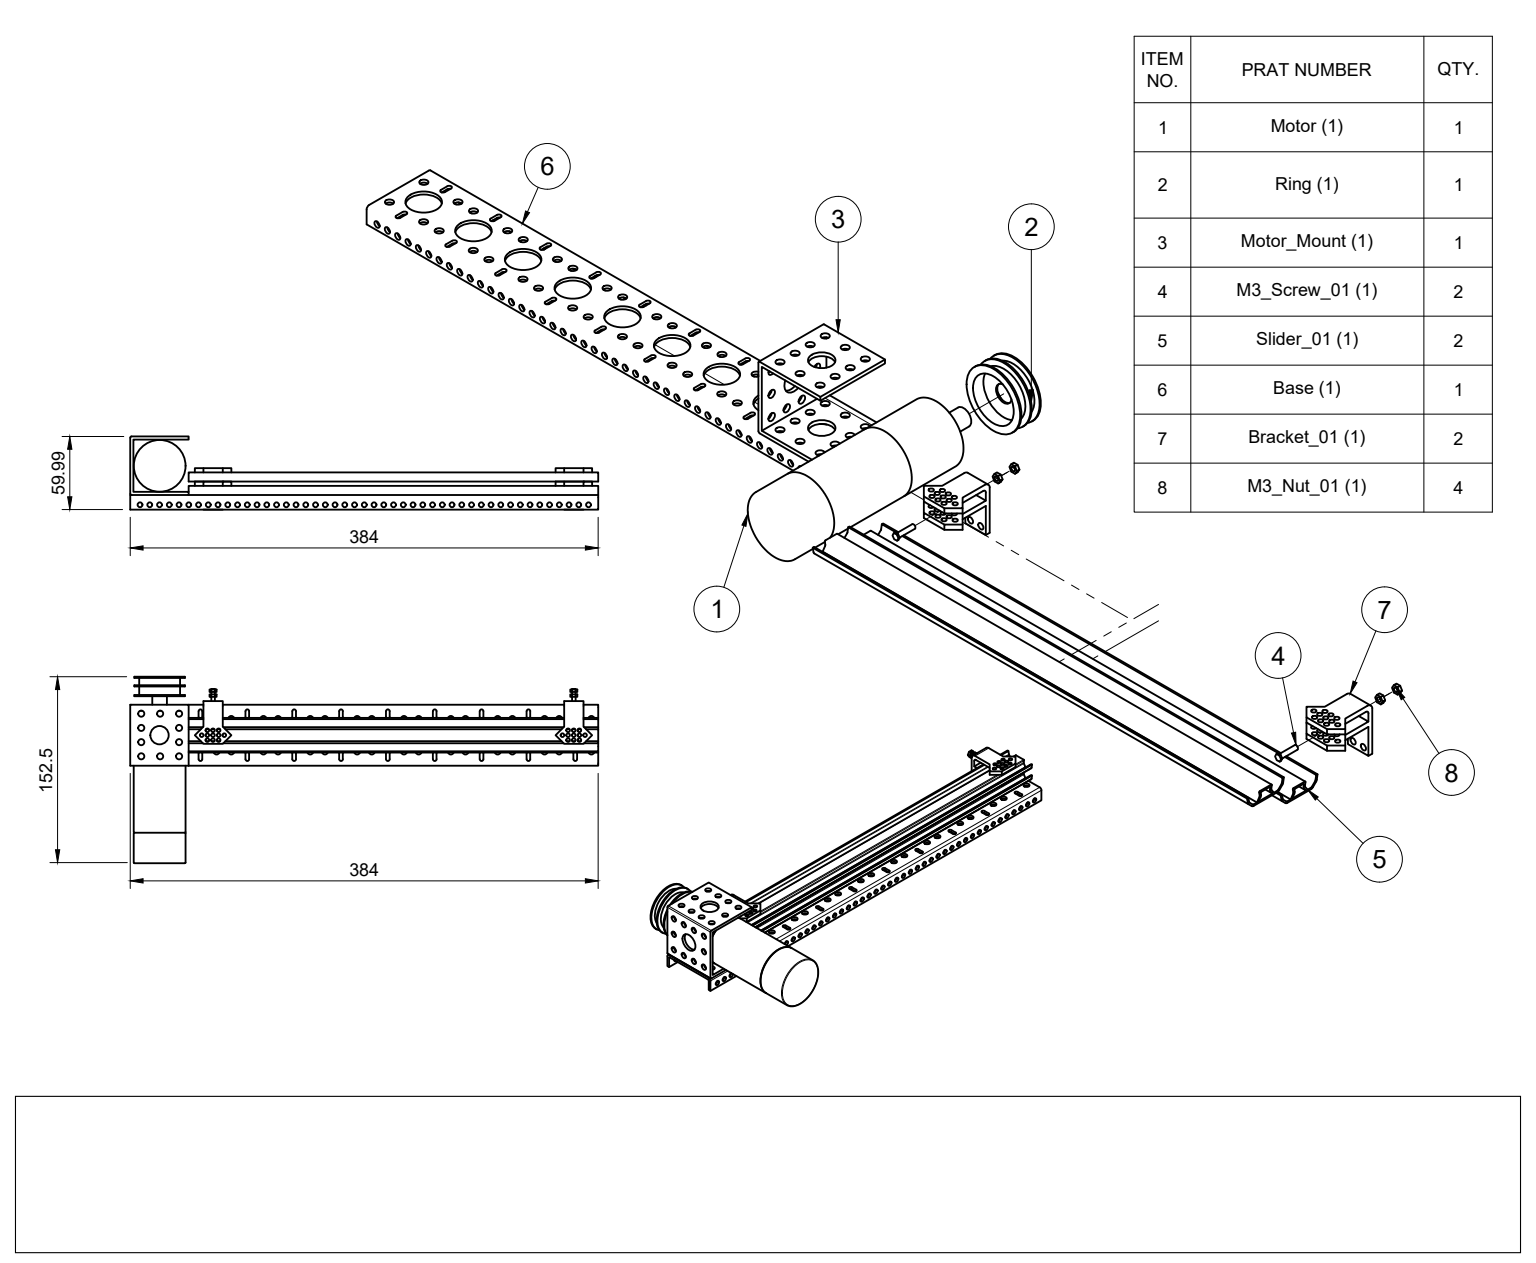
ISO-10303-21;
HEADER;
/* Generated by software containing ST-Developer
 * from STEP Tools, Inc. (www.steptools.com) 
 */

FILE_DESCRIPTION(
/* description */ (''),
/* implementation_level */ '2;1');

FILE_NAME(
/* name */ 'MAS-275',
/* time_stamp */ '2026-10-22T15:07:41+06:00',
/* author */ (''),
/* organization */ (''),
/* preprocessor_version */ 'ST-DEVELOPER v20.2',
/* originating_system */ 'Autodesk Translation Framework v15.15.0.0',
/* authorisation */ '');

FILE_SCHEMA (('AUTOMOTIVE_DESIGN { 1 0 10303 214 3 1 1 }'));
ENDSEC;

DATA;
#10=MECHANICAL_DESIGN_GEOMETRIC_PRESENTATION_REPRESENTATION('',(#2876,#2877,
#2878,#2879,#2880,#2881,#2882,#2883,#2884,#2885,#2886,#2887,#2888,#2889,
#2890,#2891),#19220);
#11=ITEM_DEFINED_TRANSFORMATION($,$,#11484,#12714);
#12=ITEM_DEFINED_TRANSFORMATION($,$,#11522,#12715);
#13=ITEM_DEFINED_TRANSFORMATION($,$,#11555,#12716);
#14=ITEM_DEFINED_TRANSFORMATION($,$,#11671,#12717);
#15=ITEM_DEFINED_TRANSFORMATION($,$,#11684,#12718);
#16=ITEM_DEFINED_TRANSFORMATION($,$,#11759,#12719);
#17=ITEM_DEFINED_TRANSFORMATION($,$,#12374,#12720);
#18=ITEM_DEFINED_TRANSFORMATION($,$,#12476,#12721);
#19=ITEM_DEFINED_TRANSFORMATION($,$,#12488,#12722);
#20=ITEM_DEFINED_TRANSFORMATION($,$,#12590,#12723);
#21=ITEM_DEFINED_TRANSFORMATION($,$,#12603,#12724);
#22=ITEM_DEFINED_TRANSFORMATION($,$,#12615,#12725);
#23=ITEM_DEFINED_TRANSFORMATION($,$,#12627,#12726);
#24=ITEM_DEFINED_TRANSFORMATION($,$,#12702,#12727);
#25=(
REPRESENTATION_RELATIONSHIP($,$,#19270,#19269)
REPRESENTATION_RELATIONSHIP_WITH_TRANSFORMATION(#11)
SHAPE_REPRESENTATION_RELATIONSHIP()
);
#26=(
REPRESENTATION_RELATIONSHIP($,$,#19271,#19269)
REPRESENTATION_RELATIONSHIP_WITH_TRANSFORMATION(#12)
SHAPE_REPRESENTATION_RELATIONSHIP()
);
#27=(
REPRESENTATION_RELATIONSHIP($,$,#19272,#19269)
REPRESENTATION_RELATIONSHIP_WITH_TRANSFORMATION(#13)
SHAPE_REPRESENTATION_RELATIONSHIP()
);
#28=(
REPRESENTATION_RELATIONSHIP($,$,#19273,#19269)
REPRESENTATION_RELATIONSHIP_WITH_TRANSFORMATION(#14)
SHAPE_REPRESENTATION_RELATIONSHIP()
);
#29=(
REPRESENTATION_RELATIONSHIP($,$,#19274,#19269)
REPRESENTATION_RELATIONSHIP_WITH_TRANSFORMATION(#15)
SHAPE_REPRESENTATION_RELATIONSHIP()
);
#30=(
REPRESENTATION_RELATIONSHIP($,$,#19275,#19269)
REPRESENTATION_RELATIONSHIP_WITH_TRANSFORMATION(#16)
SHAPE_REPRESENTATION_RELATIONSHIP()
);
#31=(
REPRESENTATION_RELATIONSHIP($,$,#19276,#19269)
REPRESENTATION_RELATIONSHIP_WITH_TRANSFORMATION(#17)
SHAPE_REPRESENTATION_RELATIONSHIP()
);
#32=(
REPRESENTATION_RELATIONSHIP($,$,#19277,#19269)
REPRESENTATION_RELATIONSHIP_WITH_TRANSFORMATION(#18)
SHAPE_REPRESENTATION_RELATIONSHIP()
);
#33=(
REPRESENTATION_RELATIONSHIP($,$,#19278,#19269)
REPRESENTATION_RELATIONSHIP_WITH_TRANSFORMATION(#19)
SHAPE_REPRESENTATION_RELATIONSHIP()
);
#34=(
REPRESENTATION_RELATIONSHIP($,$,#19279,#19269)
REPRESENTATION_RELATIONSHIP_WITH_TRANSFORMATION(#20)
SHAPE_REPRESENTATION_RELATIONSHIP()
);
#35=(
REPRESENTATION_RELATIONSHIP($,$,#19280,#19269)
REPRESENTATION_RELATIONSHIP_WITH_TRANSFORMATION(#21)
SHAPE_REPRESENTATION_RELATIONSHIP()
);
#36=(
REPRESENTATION_RELATIONSHIP($,$,#19281,#19269)
REPRESENTATION_RELATIONSHIP_WITH_TRANSFORMATION(#22)
SHAPE_REPRESENTATION_RELATIONSHIP()
);
#37=(
REPRESENTATION_RELATIONSHIP($,$,#19282,#19269)
REPRESENTATION_RELATIONSHIP_WITH_TRANSFORMATION(#23)
SHAPE_REPRESENTATION_RELATIONSHIP()
);
#38=(
REPRESENTATION_RELATIONSHIP($,$,#19283,#19269)
REPRESENTATION_RELATIONSHIP_WITH_TRANSFORMATION(#24)
SHAPE_REPRESENTATION_RELATIONSHIP()
);
#39=CONTEXT_DEPENDENT_SHAPE_REPRESENTATION(#25,#19255);
#40=CONTEXT_DEPENDENT_SHAPE_REPRESENTATION(#26,#19256);
#41=CONTEXT_DEPENDENT_SHAPE_REPRESENTATION(#27,#19257);
#42=CONTEXT_DEPENDENT_SHAPE_REPRESENTATION(#28,#19258);
#43=CONTEXT_DEPENDENT_SHAPE_REPRESENTATION(#29,#19259);
#44=CONTEXT_DEPENDENT_SHAPE_REPRESENTATION(#30,#19260);
#45=CONTEXT_DEPENDENT_SHAPE_REPRESENTATION(#31,#19261);
#46=CONTEXT_DEPENDENT_SHAPE_REPRESENTATION(#32,#19262);
#47=CONTEXT_DEPENDENT_SHAPE_REPRESENTATION(#33,#19263);
#48=CONTEXT_DEPENDENT_SHAPE_REPRESENTATION(#34,#19264);
#49=CONTEXT_DEPENDENT_SHAPE_REPRESENTATION(#35,#19265);
#50=CONTEXT_DEPENDENT_SHAPE_REPRESENTATION(#36,#19266);
#51=CONTEXT_DEPENDENT_SHAPE_REPRESENTATION(#37,#19267);
#52=CONTEXT_DEPENDENT_SHAPE_REPRESENTATION(#38,#19268);
#53=NEXT_ASSEMBLY_USAGE_OCCURRENCE('Motor (1):1','Motor (1):1',
'Motor (1):1',#19285,#19286,'Motor (1):1');
#54=NEXT_ASSEMBLY_USAGE_OCCURRENCE('Ring (1):1','Ring (1):1',
'Ring (1):1',#19285,#19287,'Ring (1):1');
#55=NEXT_ASSEMBLY_USAGE_OCCURRENCE('Motor_Mount (1):1',
'Motor_Mount (1):1','Motor_Mount (1):1',#19285,#19288,
'Motor_Mount (1):1');
#56=NEXT_ASSEMBLY_USAGE_OCCURRENCE('M3_Screw_01 (1):1',
'M3_Screw_01 (1):1','M3_Screw_01 (1):1',#19285,#19289,
'M3_Screw_01 (1):1');
#57=NEXT_ASSEMBLY_USAGE_OCCURRENCE('Slider_01 (1):1','Slider_01 (1):1',
'Slider_01 (1):1',#19285,#19290,'Slider_01 (1):1');
#58=NEXT_ASSEMBLY_USAGE_OCCURRENCE('Base (1):1','Base (1):1',
'Base (1):1',#19285,#19291,'Base (1):1');
#59=NEXT_ASSEMBLY_USAGE_OCCURRENCE('Bracket_01 (1):1',
'Bracket_01 (1):1','Bracket_01 (1):1',#19285,#19292,'Bracket_01 (1):1');
#60=NEXT_ASSEMBLY_USAGE_OCCURRENCE('M3_Nut_01 (1):1','M3_Nut_01 (1):1',
'M3_Nut_01 (1):1',#19285,#19293,'M3_Nut_01 (1):1');
#61=NEXT_ASSEMBLY_USAGE_OCCURRENCE('Bracket_02 (1):1',
'Bracket_02 (1):1','Bracket_02 (1):1',#19285,#19294,'Bracket_02 (1):1');
#62=NEXT_ASSEMBLY_USAGE_OCCURRENCE('M3_Screw_02 (1):1',
'M3_Screw_02 (1):1','M3_Screw_02 (1):1',#19285,#19295,
'M3_Screw_02 (1):1');
#63=NEXT_ASSEMBLY_USAGE_OCCURRENCE('M3_Nut_02 (1):1','M3_Nut_02 (1):1',
'M3_Nut_02 (1):1',#19285,#19296,'M3_Nut_02 (1):1');
#64=NEXT_ASSEMBLY_USAGE_OCCURRENCE('M3_Nut_03 (1):1','M3_Nut_03 (1):1',
'M3_Nut_03 (1):1',#19285,#19297,'M3_Nut_03 (1):1');
#65=NEXT_ASSEMBLY_USAGE_OCCURRENCE('Slider_02 (1):1','Slider_02 (1):1',
'Slider_02 (1):1',#19285,#19298,'Slider_02 (1):1');
#66=NEXT_ASSEMBLY_USAGE_OCCURRENCE('M3_Nut_04 (1):1','M3_Nut_04 (1):1',
'M3_Nut_04 (1):1',#19285,#19299,'M3_Nut_04 (1):1');
#67=SHAPE_REPRESENTATION_RELATIONSHIP('SRR','None',#19270,#81);
#68=SHAPE_REPRESENTATION_RELATIONSHIP('SRR','None',#19271,#82);
#69=SHAPE_REPRESENTATION_RELATIONSHIP('SRR','None',#19272,#83);
#70=SHAPE_REPRESENTATION_RELATIONSHIP('SRR','None',#19273,#84);
#71=SHAPE_REPRESENTATION_RELATIONSHIP('SRR','None',#19274,#85);
#72=SHAPE_REPRESENTATION_RELATIONSHIP('SRR','None',#19275,#86);
#73=SHAPE_REPRESENTATION_RELATIONSHIP('SRR','None',#19276,#87);
#74=SHAPE_REPRESENTATION_RELATIONSHIP('SRR','None',#19277,#88);
#75=SHAPE_REPRESENTATION_RELATIONSHIP('SRR','None',#19278,#89);
#76=SHAPE_REPRESENTATION_RELATIONSHIP('SRR','None',#19279,#90);
#77=SHAPE_REPRESENTATION_RELATIONSHIP('SRR','None',#19280,#91);
#78=SHAPE_REPRESENTATION_RELATIONSHIP('SRR','None',#19281,#92);
#79=SHAPE_REPRESENTATION_RELATIONSHIP('SRR','None',#19282,#93);
#80=SHAPE_REPRESENTATION_RELATIONSHIP('SRR','None',#19283,#94);
#81=ADVANCED_BREP_SHAPE_REPRESENTATION('',(#95),#19206);
#82=ADVANCED_BREP_SHAPE_REPRESENTATION('',(#96),#19207);
#83=ADVANCED_BREP_SHAPE_REPRESENTATION('',(#97),#19208);
#84=ADVANCED_BREP_SHAPE_REPRESENTATION('',(#98),#19209);
#85=ADVANCED_BREP_SHAPE_REPRESENTATION('',(#99),#19210);
#86=ADVANCED_BREP_SHAPE_REPRESENTATION('',(#100),#19211);
#87=ADVANCED_BREP_SHAPE_REPRESENTATION('',(#101),#19212);
#88=ADVANCED_BREP_SHAPE_REPRESENTATION('',(#102),#19213);
#89=ADVANCED_BREP_SHAPE_REPRESENTATION('',(#103),#19214);
#90=ADVANCED_BREP_SHAPE_REPRESENTATION('',(#104),#19215);
#91=ADVANCED_BREP_SHAPE_REPRESENTATION('',(#105),#19216);
#92=ADVANCED_BREP_SHAPE_REPRESENTATION('',(#106),#19217);
#93=ADVANCED_BREP_SHAPE_REPRESENTATION('',(#107),#19218);
#94=ADVANCED_BREP_SHAPE_REPRESENTATION('',(#108),#19219);
#95=MANIFOLD_SOLID_BREP('Motor',#11314);
#96=MANIFOLD_SOLID_BREP('Ring',#11315);
#97=MANIFOLD_SOLID_BREP('Motor_Mount',#11316);
#98=MANIFOLD_SOLID_BREP('M3_Screw_01',#11317);
#99=MANIFOLD_SOLID_BREP('Slider_01',#11318);
#100=MANIFOLD_SOLID_BREP('Base',#11319);
#101=MANIFOLD_SOLID_BREP('Bracket_01',#11320);
#102=MANIFOLD_SOLID_BREP('M3_Nut_01',#11321);
#103=MANIFOLD_SOLID_BREP('Bracket_02',#11322);
#104=MANIFOLD_SOLID_BREP('M3_Screw_02',#11323);
#105=MANIFOLD_SOLID_BREP('M3_Nut_02',#11324);
#106=MANIFOLD_SOLID_BREP('M3_Nut_03',#11325);
#107=MANIFOLD_SOLID_BREP('Slider_02',#11326);
#108=MANIFOLD_SOLID_BREP('M3_Nut_04',#11327);
#109=FACE_BOUND('',#3450,.T.);
#110=FACE_BOUND('',#3453,.T.);
#111=FACE_BOUND('',#3456,.T.);
#112=FACE_BOUND('',#3458,.T.);
#113=FACE_BOUND('',#3460,.T.);
#114=FACE_BOUND('',#3464,.T.);
#115=FACE_BOUND('',#3467,.T.);
#116=FACE_BOUND('',#3472,.T.);
#117=FACE_BOUND('',#3475,.T.);
#118=FACE_BOUND('',#3478,.T.);
#119=FACE_BOUND('',#3479,.T.);
#120=FACE_BOUND('',#3480,.T.);
#121=FACE_BOUND('',#3481,.T.);
#122=FACE_BOUND('',#3482,.T.);
#123=FACE_BOUND('',#3483,.T.);
#124=FACE_BOUND('',#3484,.T.);
#125=FACE_BOUND('',#3485,.T.);
#126=FACE_BOUND('',#3486,.T.);
#127=FACE_BOUND('',#3487,.T.);
#128=FACE_BOUND('',#3488,.T.);
#129=FACE_BOUND('',#3526,.T.);
#130=FACE_BOUND('',#3527,.T.);
#131=FACE_BOUND('',#3528,.T.);
#132=FACE_BOUND('',#3529,.T.);
#133=FACE_BOUND('',#3530,.T.);
#134=FACE_BOUND('',#3531,.T.);
#135=FACE_BOUND('',#3532,.T.);
#136=FACE_BOUND('',#3533,.T.);
#137=FACE_BOUND('',#3534,.T.);
#138=FACE_BOUND('',#3535,.T.);
#139=FACE_BOUND('',#3536,.T.);
#140=FACE_BOUND('',#3538,.T.);
#141=FACE_BOUND('',#3539,.T.);
#142=FACE_BOUND('',#3540,.T.);
#143=FACE_BOUND('',#3541,.T.);
#144=FACE_BOUND('',#3542,.T.);
#145=FACE_BOUND('',#3543,.T.);
#146=FACE_BOUND('',#3544,.T.);
#147=FACE_BOUND('',#3545,.T.);
#148=FACE_BOUND('',#3546,.T.);
#149=FACE_BOUND('',#3547,.T.);
#150=FACE_BOUND('',#3548,.T.);
#151=FACE_BOUND('',#3551,.T.);
#152=FACE_BOUND('',#3552,.T.);
#153=FACE_BOUND('',#3553,.T.);
#154=FACE_BOUND('',#3554,.T.);
#155=FACE_BOUND('',#3555,.T.);
#156=FACE_BOUND('',#3556,.T.);
#157=FACE_BOUND('',#3557,.T.);
#158=FACE_BOUND('',#3558,.T.);
#159=FACE_BOUND('',#3559,.T.);
#160=FACE_BOUND('',#3560,.T.);
#161=FACE_BOUND('',#3561,.T.);
#162=FACE_BOUND('',#3563,.T.);
#163=FACE_BOUND('',#3564,.T.);
#164=FACE_BOUND('',#3565,.T.);
#165=FACE_BOUND('',#3566,.T.);
#166=FACE_BOUND('',#3567,.T.);
#167=FACE_BOUND('',#3568,.T.);
#168=FACE_BOUND('',#3569,.T.);
#169=FACE_BOUND('',#3570,.T.);
#170=FACE_BOUND('',#3571,.T.);
#171=FACE_BOUND('',#3572,.T.);
#172=FACE_BOUND('',#3573,.T.);
#173=FACE_BOUND('',#3575,.T.);
#174=FACE_BOUND('',#3576,.T.);
#175=FACE_BOUND('',#3577,.T.);
#176=FACE_BOUND('',#3578,.T.);
#177=FACE_BOUND('',#3579,.T.);
#178=FACE_BOUND('',#3580,.T.);
#179=FACE_BOUND('',#3581,.T.);
#180=FACE_BOUND('',#3582,.T.);
#181=FACE_BOUND('',#3583,.T.);
#182=FACE_BOUND('',#3584,.T.);
#183=FACE_BOUND('',#3585,.T.);
#184=FACE_BOUND('',#3588,.T.);
#185=FACE_BOUND('',#3639,.T.);
#186=FACE_BOUND('',#3641,.T.);
#187=FACE_BOUND('',#3774,.T.);
#188=FACE_BOUND('',#3775,.T.);
#189=FACE_BOUND('',#3776,.T.);
#190=FACE_BOUND('',#3777,.T.);
#191=FACE_BOUND('',#3778,.T.);
#192=FACE_BOUND('',#3779,.T.);
#193=FACE_BOUND('',#3780,.T.);
#194=FACE_BOUND('',#3781,.T.);
#195=FACE_BOUND('',#3782,.T.);
#196=FACE_BOUND('',#3783,.T.);
#197=FACE_BOUND('',#3784,.T.);
#198=FACE_BOUND('',#3785,.T.);
#199=FACE_BOUND('',#3786,.T.);
#200=FACE_BOUND('',#3787,.T.);
#201=FACE_BOUND('',#3788,.T.);
#202=FACE_BOUND('',#3789,.T.);
#203=FACE_BOUND('',#3790,.T.);
#204=FACE_BOUND('',#3791,.T.);
#205=FACE_BOUND('',#3792,.T.);
#206=FACE_BOUND('',#3793,.T.);
#207=FACE_BOUND('',#3794,.T.);
#208=FACE_BOUND('',#3795,.T.);
#209=FACE_BOUND('',#3796,.T.);
#210=FACE_BOUND('',#3797,.T.);
#211=FACE_BOUND('',#3798,.T.);
#212=FACE_BOUND('',#3799,.T.);
#213=FACE_BOUND('',#3800,.T.);
#214=FACE_BOUND('',#3801,.T.);
#215=FACE_BOUND('',#3802,.T.);
#216=FACE_BOUND('',#3803,.T.);
#217=FACE_BOUND('',#3804,.T.);
#218=FACE_BOUND('',#3805,.T.);
#219=FACE_BOUND('',#3806,.T.);
#220=FACE_BOUND('',#3807,.T.);
#221=FACE_BOUND('',#3808,.T.);
#222=FACE_BOUND('',#3809,.T.);
#223=FACE_BOUND('',#3810,.T.);
#224=FACE_BOUND('',#3811,.T.);
#225=FACE_BOUND('',#3812,.T.);
#226=FACE_BOUND('',#3813,.T.);
#227=FACE_BOUND('',#3814,.T.);
#228=FACE_BOUND('',#3815,.T.);
#229=FACE_BOUND('',#3816,.T.);
#230=FACE_BOUND('',#3817,.T.);
#231=FACE_BOUND('',#3818,.T.);
#232=FACE_BOUND('',#3819,.T.);
#233=FACE_BOUND('',#3820,.T.);
#234=FACE_BOUND('',#3821,.T.);
#235=FACE_BOUND('',#3822,.T.);
#236=FACE_BOUND('',#3823,.T.);
#237=FACE_BOUND('',#3824,.T.);
#238=FACE_BOUND('',#3825,.T.);
#239=FACE_BOUND('',#3826,.T.);
#240=FACE_BOUND('',#3827,.T.);
#241=FACE_BOUND('',#3828,.T.);
#242=FACE_BOUND('',#3829,.T.);
#243=FACE_BOUND('',#3830,.T.);
#244=FACE_BOUND('',#3831,.T.);
#245=FACE_BOUND('',#3832,.T.);
#246=FACE_BOUND('',#3833,.T.);
#247=FACE_BOUND('',#3834,.T.);
#248=FACE_BOUND('',#3835,.T.);
#249=FACE_BOUND('',#3836,.T.);
#250=FACE_BOUND('',#3837,.T.);
#251=FACE_BOUND('',#3838,.T.);
#252=FACE_BOUND('',#3839,.T.);
#253=FACE_BOUND('',#3840,.T.);
#254=FACE_BOUND('',#3841,.T.);
#255=FACE_BOUND('',#3842,.T.);
#256=FACE_BOUND('',#3843,.T.);
#257=FACE_BOUND('',#3846,.T.);
#258=FACE_BOUND('',#3847,.T.);
#259=FACE_BOUND('',#3848,.T.);
#260=FACE_BOUND('',#3849,.T.);
#261=FACE_BOUND('',#3850,.T.);
#262=FACE_BOUND('',#3851,.T.);
#263=FACE_BOUND('',#3852,.T.);
#264=FACE_BOUND('',#3853,.T.);
#265=FACE_BOUND('',#3854,.T.);
#266=FACE_BOUND('',#3855,.T.);
#267=FACE_BOUND('',#3856,.T.);
#268=FACE_BOUND('',#3857,.T.);
#269=FACE_BOUND('',#3858,.T.);
#270=FACE_BOUND('',#3859,.T.);
#271=FACE_BOUND('',#3860,.T.);
#272=FACE_BOUND('',#3861,.T.);
#273=FACE_BOUND('',#3862,.T.);
#274=FACE_BOUND('',#3863,.T.);
#275=FACE_BOUND('',#3864,.T.);
#276=FACE_BOUND('',#3865,.T.);
#277=FACE_BOUND('',#3866,.T.);
#278=FACE_BOUND('',#3867,.T.);
#279=FACE_BOUND('',#3868,.T.);
#280=FACE_BOUND('',#3869,.T.);
#281=FACE_BOUND('',#3870,.T.);
#282=FACE_BOUND('',#3871,.T.);
#283=FACE_BOUND('',#3872,.T.);
#284=FACE_BOUND('',#3873,.T.);
#285=FACE_BOUND('',#3874,.T.);
#286=FACE_BOUND('',#3875,.T.);
#287=FACE_BOUND('',#3876,.T.);
#288=FACE_BOUND('',#3877,.T.);
#289=FACE_BOUND('',#3878,.T.);
#290=FACE_BOUND('',#3879,.T.);
#291=FACE_BOUND('',#3880,.T.);
#292=FACE_BOUND('',#3881,.T.);
#293=FACE_BOUND('',#3882,.T.);
#294=FACE_BOUND('',#3883,.T.);
#295=FACE_BOUND('',#3884,.T.);
#296=FACE_BOUND('',#3885,.T.);
#297=FACE_BOUND('',#3886,.T.);
#298=FACE_BOUND('',#3887,.T.);
#299=FACE_BOUND('',#3888,.T.);
#300=FACE_BOUND('',#3889,.T.);
#301=FACE_BOUND('',#3890,.T.);
#302=FACE_BOUND('',#3891,.T.);
#303=FACE_BOUND('',#3892,.T.);
#304=FACE_BOUND('',#3895,.T.);
#305=FACE_BOUND('',#3896,.T.);
#306=FACE_BOUND('',#3897,.T.);
#307=FACE_BOUND('',#3898,.T.);
#308=FACE_BOUND('',#3899,.T.);
#309=FACE_BOUND('',#3900,.T.);
#310=FACE_BOUND('',#3901,.T.);
#311=FACE_BOUND('',#3902,.T.);
#312=FACE_BOUND('',#3903,.T.);
#313=FACE_BOUND('',#3904,.T.);
#314=FACE_BOUND('',#3905,.T.);
#315=FACE_BOUND('',#3906,.T.);
#316=FACE_BOUND('',#3907,.T.);
#317=FACE_BOUND('',#3908,.T.);
#318=FACE_BOUND('',#3909,.T.);
#319=FACE_BOUND('',#3910,.T.);
#320=FACE_BOUND('',#3911,.T.);
#321=FACE_BOUND('',#3912,.T.);
#322=FACE_BOUND('',#3913,.T.);
#323=FACE_BOUND('',#3914,.T.);
#324=FACE_BOUND('',#3915,.T.);
#325=FACE_BOUND('',#3916,.T.);
#326=FACE_BOUND('',#3917,.T.);
#327=FACE_BOUND('',#3918,.T.);
#328=FACE_BOUND('',#3919,.T.);
#329=FACE_BOUND('',#3920,.T.);
#330=FACE_BOUND('',#3921,.T.);
#331=FACE_BOUND('',#3922,.T.);
#332=FACE_BOUND('',#3923,.T.);
#333=FACE_BOUND('',#3924,.T.);
#334=FACE_BOUND('',#3925,.T.);
#335=FACE_BOUND('',#3926,.T.);
#336=FACE_BOUND('',#3927,.T.);
#337=FACE_BOUND('',#3928,.T.);
#338=FACE_BOUND('',#3929,.T.);
#339=FACE_BOUND('',#3930,.T.);
#340=FACE_BOUND('',#3931,.T.);
#341=FACE_BOUND('',#3932,.T.);
#342=FACE_BOUND('',#3933,.T.);
#343=FACE_BOUND('',#3934,.T.);
#344=FACE_BOUND('',#3935,.T.);
#345=FACE_BOUND('',#3936,.T.);
#346=FACE_BOUND('',#3937,.T.);
#347=FACE_BOUND('',#3938,.T.);
#348=FACE_BOUND('',#3939,.T.);
#349=FACE_BOUND('',#3940,.T.);
#350=FACE_BOUND('',#3941,.T.);
#351=FACE_BOUND('',#3942,.T.);
#352=FACE_BOUND('',#3943,.T.);
#353=FACE_BOUND('',#3944,.T.);
#354=FACE_BOUND('',#3945,.T.);
#355=FACE_BOUND('',#3946,.T.);
#356=FACE_BOUND('',#3947,.T.);
#357=FACE_BOUND('',#3948,.T.);
#358=FACE_BOUND('',#3949,.T.);
#359=FACE_BOUND('',#3950,.T.);
#360=FACE_BOUND('',#3951,.T.);
#361=FACE_BOUND('',#3952,.T.);
#362=FACE_BOUND('',#3953,.T.);
#363=FACE_BOUND('',#3954,.T.);
#364=FACE_BOUND('',#3955,.T.);
#365=FACE_BOUND('',#3956,.T.);
#366=FACE_BOUND('',#3957,.T.);
#367=FACE_BOUND('',#3958,.T.);
#368=FACE_BOUND('',#3959,.T.);
#369=FACE_BOUND('',#3960,.T.);
#370=FACE_BOUND('',#3961,.T.);
#371=FACE_BOUND('',#3962,.T.);
#372=FACE_BOUND('',#3963,.T.);
#373=FACE_BOUND('',#3964,.T.);
#374=FACE_BOUND('',#4016,.T.);
#375=FACE_BOUND('',#4017,.T.);
#376=FACE_BOUND('',#4018,.T.);
#377=FACE_BOUND('',#4019,.T.);
#378=FACE_BOUND('',#4020,.T.);
#379=FACE_BOUND('',#4021,.T.);
#380=FACE_BOUND('',#4022,.T.);
#381=FACE_BOUND('',#4023,.T.);
#382=FACE_BOUND('',#4024,.T.);
#383=FACE_BOUND('',#4025,.T.);
#384=FACE_BOUND('',#4026,.T.);
#385=FACE_BOUND('',#4027,.T.);
#386=FACE_BOUND('',#4028,.T.);
#387=FACE_BOUND('',#4029,.T.);
#388=FACE_BOUND('',#4030,.T.);
#389=FACE_BOUND('',#4031,.T.);
#390=FACE_BOUND('',#4032,.T.);
#391=FACE_BOUND('',#4033,.T.);
#392=FACE_BOUND('',#4034,.T.);
#393=FACE_BOUND('',#4035,.T.);
#394=FACE_BOUND('',#4036,.T.);
#395=FACE_BOUND('',#4037,.T.);
#396=FACE_BOUND('',#4038,.T.);
#397=FACE_BOUND('',#4039,.T.);
#398=FACE_BOUND('',#4040,.T.);
#399=FACE_BOUND('',#4041,.T.);
#400=FACE_BOUND('',#4042,.T.);
#401=FACE_BOUND('',#4043,.T.);
#402=FACE_BOUND('',#4044,.T.);
#403=FACE_BOUND('',#4045,.T.);
#404=FACE_BOUND('',#4046,.T.);
#405=FACE_BOUND('',#4047,.T.);
#406=FACE_BOUND('',#4048,.T.);
#407=FACE_BOUND('',#4049,.T.);
#408=FACE_BOUND('',#4050,.T.);
#409=FACE_BOUND('',#4051,.T.);
#410=FACE_BOUND('',#4052,.T.);
#411=FACE_BOUND('',#4053,.T.);
#412=FACE_BOUND('',#4054,.T.);
#413=FACE_BOUND('',#4055,.T.);
#414=FACE_BOUND('',#4056,.T.);
#415=FACE_BOUND('',#4057,.T.);
#416=FACE_BOUND('',#4058,.T.);
#417=FACE_BOUND('',#4059,.T.);
#418=FACE_BOUND('',#4060,.T.);
#419=FACE_BOUND('',#4061,.T.);
#420=FACE_BOUND('',#4062,.T.);
#421=FACE_BOUND('',#4113,.T.);
#422=FACE_BOUND('',#4114,.T.);
#423=FACE_BOUND('',#4115,.T.);
#424=FACE_BOUND('',#4116,.T.);
#425=FACE_BOUND('',#4117,.T.);
#426=FACE_BOUND('',#4118,.T.);
#427=FACE_BOUND('',#4119,.T.);
#428=FACE_BOUND('',#4120,.T.);
#429=FACE_BOUND('',#4121,.T.);
#430=FACE_BOUND('',#4122,.T.);
#431=FACE_BOUND('',#4123,.T.);
#432=FACE_BOUND('',#4124,.T.);
#433=FACE_BOUND('',#4125,.T.);
#434=FACE_BOUND('',#4126,.T.);
#435=FACE_BOUND('',#4127,.T.);
#436=FACE_BOUND('',#4128,.T.);
#437=FACE_BOUND('',#4129,.T.);
#438=FACE_BOUND('',#4130,.T.);
#439=FACE_BOUND('',#4131,.T.);
#440=FACE_BOUND('',#4132,.T.);
#441=FACE_BOUND('',#4133,.T.);
#442=FACE_BOUND('',#4134,.T.);
#443=FACE_BOUND('',#4135,.T.);
#444=FACE_BOUND('',#4136,.T.);
#445=FACE_BOUND('',#4137,.T.);
#446=FACE_BOUND('',#4138,.T.);
#447=FACE_BOUND('',#4139,.T.);
#448=FACE_BOUND('',#4140,.T.);
#449=FACE_BOUND('',#4141,.T.);
#450=FACE_BOUND('',#4142,.T.);
#451=FACE_BOUND('',#4143,.T.);
#452=FACE_BOUND('',#4144,.T.);
#453=FACE_BOUND('',#4145,.T.);
#454=FACE_BOUND('',#4146,.T.);
#455=FACE_BOUND('',#4147,.T.);
#456=FACE_BOUND('',#4148,.T.);
#457=FACE_BOUND('',#4149,.T.);
#458=FACE_BOUND('',#4150,.T.);
#459=FACE_BOUND('',#4151,.T.);
#460=FACE_BOUND('',#4152,.T.);
#461=FACE_BOUND('',#4153,.T.);
#462=FACE_BOUND('',#4154,.T.);
#463=FACE_BOUND('',#4155,.T.);
#464=FACE_BOUND('',#4156,.T.);
#465=FACE_BOUND('',#4157,.T.);
#466=FACE_BOUND('',#4158,.T.);
#467=FACE_BOUND('',#4159,.T.);
#468=FACE_BOUND('',#4161,.T.);
#469=FACE_BOUND('',#4162,.T.);
#470=FACE_BOUND('',#4163,.T.);
#471=FACE_BOUND('',#4164,.T.);
#472=FACE_BOUND('',#4165,.T.);
#473=FACE_BOUND('',#4166,.T.);
#474=FACE_BOUND('',#4167,.T.);
#475=FACE_BOUND('',#4168,.T.);
#476=FACE_BOUND('',#4169,.T.);
#477=FACE_BOUND('',#4170,.T.);
#478=FACE_BOUND('',#4171,.T.);
#479=FACE_BOUND('',#4172,.T.);
#480=FACE_BOUND('',#4173,.T.);
#481=FACE_BOUND('',#4174,.T.);
#482=FACE_BOUND('',#4175,.T.);
#483=FACE_BOUND('',#4176,.T.);
#484=FACE_BOUND('',#4177,.T.);
#485=FACE_BOUND('',#4178,.T.);
#486=FACE_BOUND('',#4179,.T.);
#487=FACE_BOUND('',#4180,.T.);
#488=FACE_BOUND('',#4181,.T.);
#489=FACE_BOUND('',#4182,.T.);
#490=FACE_BOUND('',#4183,.T.);
#491=FACE_BOUND('',#4184,.T.);
#492=FACE_BOUND('',#4185,.T.);
#493=FACE_BOUND('',#4186,.T.);
#494=FACE_BOUND('',#4187,.T.);
#495=FACE_BOUND('',#4188,.T.);
#496=FACE_BOUND('',#4189,.T.);
#497=FACE_BOUND('',#4190,.T.);
#498=FACE_BOUND('',#4191,.T.);
#499=FACE_BOUND('',#4192,.T.);
#500=FACE_BOUND('',#4193,.T.);
#501=FACE_BOUND('',#4194,.T.);
#502=FACE_BOUND('',#4195,.T.);
#503=FACE_BOUND('',#4196,.T.);
#504=FACE_BOUND('',#4197,.T.);
#505=FACE_BOUND('',#4198,.T.);
#506=FACE_BOUND('',#4199,.T.);
#507=FACE_BOUND('',#4200,.T.);
#508=FACE_BOUND('',#4201,.T.);
#509=FACE_BOUND('',#4202,.T.);
#510=FACE_BOUND('',#4203,.T.);
#511=FACE_BOUND('',#4204,.T.);
#512=FACE_BOUND('',#4205,.T.);
#513=FACE_BOUND('',#4206,.T.);
#514=FACE_BOUND('',#4207,.T.);
#515=FACE_BOUND('',#4213,.T.);
#516=FACE_BOUND('',#4214,.T.);
#517=FACE_BOUND('',#4215,.T.);
#518=FACE_BOUND('',#4216,.T.);
#519=FACE_BOUND('',#4217,.T.);
#520=FACE_BOUND('',#4218,.T.);
#521=FACE_BOUND('',#4219,.T.);
#522=FACE_BOUND('',#4220,.T.);
#523=FACE_BOUND('',#4221,.T.);
#524=FACE_BOUND('',#4222,.T.);
#525=FACE_BOUND('',#4223,.T.);
#526=FACE_BOUND('',#4226,.T.);
#527=FACE_BOUND('',#4227,.T.);
#528=FACE_BOUND('',#4228,.T.);
#529=FACE_BOUND('',#4229,.T.);
#530=FACE_BOUND('',#4230,.T.);
#531=FACE_BOUND('',#4231,.T.);
#532=FACE_BOUND('',#4232,.T.);
#533=FACE_BOUND('',#4233,.T.);
#534=FACE_BOUND('',#4234,.T.);
#535=FACE_BOUND('',#4235,.T.);
#536=FACE_BOUND('',#4236,.T.);
#537=FACE_BOUND('',#4254,.T.);
#538=FACE_BOUND('',#4255,.T.);
#539=FACE_BOUND('',#4256,.T.);
#540=FACE_BOUND('',#4257,.T.);
#541=FACE_BOUND('',#4258,.T.);
#542=FACE_BOUND('',#4259,.T.);
#543=FACE_BOUND('',#4260,.T.);
#544=FACE_BOUND('',#4261,.T.);
#545=FACE_BOUND('',#4262,.T.);
#546=FACE_BOUND('',#4263,.T.);
#547=FACE_BOUND('',#4264,.T.);
#548=FACE_BOUND('',#4282,.T.);
#549=FACE_BOUND('',#4283,.T.);
#550=FACE_BOUND('',#4284,.T.);
#551=FACE_BOUND('',#4285,.T.);
#552=FACE_BOUND('',#4286,.T.);
#553=FACE_BOUND('',#4287,.T.);
#554=FACE_BOUND('',#4288,.T.);
#555=FACE_BOUND('',#4289,.T.);
#556=FACE_BOUND('',#4290,.T.);
#557=FACE_BOUND('',#4291,.T.);
#558=FACE_BOUND('',#4292,.T.);
#559=FACE_BOUND('',#4294,.T.);
#560=FACE_BOUND('',#4295,.T.);
#561=FACE_BOUND('',#4296,.T.);
#562=FACE_BOUND('',#4298,.T.);
#563=FACE_BOUND('',#4301,.T.);
#564=FACE_BOUND('',#4302,.T.);
#565=FACE_BOUND('',#4313,.T.);
#566=FACE_BOUND('',#4315,.T.);
#567=FACE_BOUND('',#4321,.T.);
#568=FACE_BOUND('',#4322,.T.);
#569=FACE_BOUND('',#4323,.T.);
#570=FACE_BOUND('',#4324,.T.);
#571=FACE_BOUND('',#4325,.T.);
#572=FACE_BOUND('',#4326,.T.);
#573=FACE_BOUND('',#4327,.T.);
#574=FACE_BOUND('',#4328,.T.);
#575=FACE_BOUND('',#4329,.T.);
#576=FACE_BOUND('',#4330,.T.);
#577=FACE_BOUND('',#4331,.T.);
#578=FACE_BOUND('',#4334,.T.);
#579=FACE_BOUND('',#4335,.T.);
#580=FACE_BOUND('',#4336,.T.);
#581=FACE_BOUND('',#4337,.T.);
#582=FACE_BOUND('',#4338,.T.);
#583=FACE_BOUND('',#4339,.T.);
#584=FACE_BOUND('',#4340,.T.);
#585=FACE_BOUND('',#4341,.T.);
#586=FACE_BOUND('',#4342,.T.);
#587=FACE_BOUND('',#4343,.T.);
#588=FACE_BOUND('',#4344,.T.);
#589=FACE_BOUND('',#4362,.T.);
#590=FACE_BOUND('',#4363,.T.);
#591=FACE_BOUND('',#4364,.T.);
#592=FACE_BOUND('',#4365,.T.);
#593=FACE_BOUND('',#4366,.T.);
#594=FACE_BOUND('',#4367,.T.);
#595=FACE_BOUND('',#4368,.T.);
#596=FACE_BOUND('',#4369,.T.);
#597=FACE_BOUND('',#4370,.T.);
#598=FACE_BOUND('',#4371,.T.);
#599=FACE_BOUND('',#4372,.T.);
#600=FACE_BOUND('',#4390,.T.);
#601=FACE_BOUND('',#4391,.T.);
#602=FACE_BOUND('',#4392,.T.);
#603=FACE_BOUND('',#4393,.T.);
#604=FACE_BOUND('',#4394,.T.);
#605=FACE_BOUND('',#4395,.T.);
#606=FACE_BOUND('',#4396,.T.);
#607=FACE_BOUND('',#4397,.T.);
#608=FACE_BOUND('',#4398,.T.);
#609=FACE_BOUND('',#4399,.T.);
#610=FACE_BOUND('',#4400,.T.);
#611=FACE_BOUND('',#4402,.T.);
#612=FACE_BOUND('',#4403,.T.);
#613=FACE_BOUND('',#4404,.T.);
#614=FACE_BOUND('',#4406,.T.);
#615=FACE_BOUND('',#4409,.T.);
#616=FACE_BOUND('',#4410,.T.);
#617=FACE_BOUND('',#4414,.T.);
#618=FACE_BOUND('',#4432,.T.);
#619=FACE_BOUND('',#4434,.T.);
#620=FACE_BOUND('',#4443,.T.);
#621=FACE_BOUND('',#4445,.T.);
#622=FACE_BOUND('',#4487,.T.);
#623=FACE_BOUND('',#4489,.T.);
#624=FACE_BOUND('',#4498,.T.);
#625=FACE_BOUND('',#4500,.T.);
#626=PLANE('',#11493);
#627=PLANE('',#11507);
#628=PLANE('',#11519);
#629=PLANE('',#11523);
#630=PLANE('',#11528);
#631=PLANE('',#11530);
#632=PLANE('',#11533);
#633=PLANE('',#11538);
#634=PLANE('',#11543);
#635=PLANE('',#11550);
#636=PLANE('',#11554);
#637=PLANE('',#11559);
#638=PLANE('',#11571);
#639=PLANE('',#11663);
#640=PLANE('',#11664);
#641=PLANE('',#11665);
#642=PLANE('',#11666);
#643=PLANE('',#11667);
#644=PLANE('',#11668);
#645=PLANE('',#11669);
#646=PLANE('',#11670);
#647=PLANE('',#11672);
#648=PLANE('',#11674);
#649=PLANE('',#11675);
#650=PLANE('',#11676);
#651=PLANE('',#11677);
#652=PLANE('',#11678);
#653=PLANE('',#11679);
#654=PLANE('',#11680);
#655=PLANE('',#11683);
#656=PLANE('',#11685);
#657=PLANE('',#11689);
#658=PLANE('',#11690);
#659=PLANE('',#11694);
#660=PLANE('',#11701);
#661=PLANE('',#11702);
#662=PLANE('',#11706);
#663=PLANE('',#11707);
#664=PLANE('',#11711);
#665=PLANE('',#11715);
#666=PLANE('',#11719);
#667=PLANE('',#11720);
#668=PLANE('',#11721);
#669=PLANE('',#11725);
#670=PLANE('',#11729);
#671=PLANE('',#11730);
#672=PLANE('',#11731);
#673=PLANE('',#11735);
#674=PLANE('',#11739);
#675=PLANE('',#11743);
#676=PLANE('',#11747);
#677=PLANE('',#11748);
#678=PLANE('',#11749);
#679=PLANE('',#11753);
#680=PLANE('',#11757);
#681=PLANE('',#11758);
#682=PLANE('',#11775);
#683=PLANE('',#11779);
#684=PLANE('',#11783);
#685=PLANE('',#11787);
#686=PLANE('',#11806);
#687=PLANE('',#11810);
#688=PLANE('',#11814);
#689=PLANE('',#11818);
#690=PLANE('',#11837);
#691=PLANE('',#11841);
#692=PLANE('',#11845);
#693=PLANE('',#11849);
#694=PLANE('',#11868);
#695=PLANE('',#11872);
#696=PLANE('',#11876);
#697=PLANE('',#11880);
#698=PLANE('',#11899);
#699=PLANE('',#11903);
#700=PLANE('',#11907);
#701=PLANE('',#11911);
#702=PLANE('',#11930);
#703=PLANE('',#11934);
#704=PLANE('',#11938);
#705=PLANE('',#11942);
#706=PLANE('',#11961);
#707=PLANE('',#11965);
#708=PLANE('',#11969);
#709=PLANE('',#11973);
#710=PLANE('',#11992);
#711=PLANE('',#11996);
#712=PLANE('',#12000);
#713=PLANE('',#12004);
#714=PLANE('',#12023);
#715=PLANE('',#12027);
#716=PLANE('',#12031);
#717=PLANE('',#12035);
#718=PLANE('',#12045);
#719=PLANE('',#12049);
#720=PLANE('',#12053);
#721=PLANE('',#12057);
#722=PLANE('',#12073);
#723=PLANE('',#12077);
#724=PLANE('',#12128);
#725=PLANE('',#12129);
#726=PLANE('',#12227);
#727=PLANE('',#12228);
#728=PLANE('',#12370);
#729=PLANE('',#12371);
#730=PLANE('',#12372);
#731=PLANE('',#12373);
#732=PLANE('',#12387);
#733=PLANE('',#12402);
#734=PLANE('',#12425);
#735=PLANE('',#12426);
#736=PLANE('',#12427);
#737=PLANE('',#12428);
#738=PLANE('',#12429);
#739=PLANE('',#12430);
#740=PLANE('',#12464);
#741=PLANE('',#12465);
#742=PLANE('',#12466);
#743=PLANE('',#12467);
#744=PLANE('',#12468);
#745=PLANE('',#12469);
#746=PLANE('',#12470);
#747=PLANE('',#12471);
#748=PLANE('',#12472);
#749=PLANE('',#12473);
#750=PLANE('',#12474);
#751=PLANE('',#12475);
#752=PLANE('',#12480);
#753=PLANE('',#12481);
#754=PLANE('',#12482);
#755=PLANE('',#12483);
#756=PLANE('',#12484);
#757=PLANE('',#12485);
#758=PLANE('',#12486);
#759=PLANE('',#12487);
#760=PLANE('',#12501);
#761=PLANE('',#12516);
#762=PLANE('',#12539);
#763=PLANE('',#12540);
#764=PLANE('',#12541);
#765=PLANE('',#12542);
#766=PLANE('',#12543);
#767=PLANE('',#12544);
#768=PLANE('',#12578);
#769=PLANE('',#12579);
#770=PLANE('',#12580);
#771=PLANE('',#12581);
#772=PLANE('',#12582);
#773=PLANE('',#12583);
#774=PLANE('',#12584);
#775=PLANE('',#12585);
#776=PLANE('',#12586);
#777=PLANE('',#12587);
#778=PLANE('',#12588);
#779=PLANE('',#12589);
#780=PLANE('',#12591);
#781=PLANE('',#12593);
#782=PLANE('',#12594);
#783=PLANE('',#12595);
#784=PLANE('',#12596);
#785=PLANE('',#12597);
#786=PLANE('',#12598);
#787=PLANE('',#12599);
#788=PLANE('',#12602);
#789=PLANE('',#12607);
#790=PLANE('',#12608);
#791=PLANE('',#12609);
#792=PLANE('',#12610);
#793=PLANE('',#12611);
#794=PLANE('',#12612);
#795=PLANE('',#12613);
#796=PLANE('',#12614);
#797=PLANE('',#12619);
#798=PLANE('',#12620);
#799=PLANE('',#12621);
#800=PLANE('',#12622);
#801=PLANE('',#12623);
#802=PLANE('',#12624);
#803=PLANE('',#12625);
#804=PLANE('',#12626);
#805=PLANE('',#12628);
#806=PLANE('',#12632);
#807=PLANE('',#12633);
#808=PLANE('',#12637);
#809=PLANE('',#12644);
#810=PLANE('',#12645);
#811=PLANE('',#12649);
#812=PLANE('',#12650);
#813=PLANE('',#12654);
#814=PLANE('',#12658);
#815=PLANE('',#12662);
#816=PLANE('',#12663);
#817=PLANE('',#12664);
#818=PLANE('',#12668);
#819=PLANE('',#12672);
#820=PLANE('',#12673);
#821=PLANE('',#12674);
#822=PLANE('',#12678);
#823=PLANE('',#12682);
#824=PLANE('',#12686);
#825=PLANE('',#12690);
#826=PLANE('',#12691);
#827=PLANE('',#12692);
#828=PLANE('',#12696);
#829=PLANE('',#12700);
#830=PLANE('',#12701);
#831=PLANE('',#12706);
#832=PLANE('',#12707);
#833=PLANE('',#12708);
#834=PLANE('',#12709);
#835=PLANE('',#12710);
#836=PLANE('',#12711);
#837=PLANE('',#12712);
#838=PLANE('',#12713);
#839=LINE('',#16085,#1694);
#840=LINE('',#16106,#1695);
#841=LINE('',#16115,#1696);
#842=LINE('',#16127,#1697);
#843=LINE('',#16142,#1698);
#844=LINE('',#16158,#1699);
#845=LINE('',#16160,#1700);
#846=LINE('',#16169,#1701);
#847=LINE('',#16175,#1702);
#848=LINE('',#16180,#1703);
#849=LINE('',#16182,#1704);
#850=LINE('',#16189,#1705);
#851=LINE('',#16197,#1706);
#852=LINE('',#16200,#1707);
#853=LINE('',#16203,#1708);
#854=LINE('',#16205,#1709);
#855=LINE('',#16206,#1710);
#856=LINE('',#16231,#1711);
#857=LINE('',#16233,#1712);
#858=LINE('',#16235,#1713);
#859=LINE('',#16237,#1714);
#860=LINE('',#16239,#1715);
#861=LINE('',#16241,#1716);
#862=LINE('',#16243,#1717);
#863=LINE('',#16248,#1718);
#864=LINE('',#16253,#1719);
#865=LINE('',#16259,#1720);
#866=LINE('',#16265,#1721);
#867=LINE('',#16271,#1722);
#868=LINE('',#16277,#1723);
#869=LINE('',#16283,#1724);
#870=LINE('',#16289,#1725);
#871=LINE('',#16295,#1726);
#872=LINE('',#16301,#1727);
#873=LINE('',#16307,#1728);
#874=LINE('',#16313,#1729);
#875=LINE('',#16317,#1730);
#876=LINE('',#16321,#1731);
#877=LINE('',#16325,#1732);
#878=LINE('',#16329,#1733);
#879=LINE('',#16333,#1734);
#880=LINE('',#16337,#1735);
#881=LINE('',#16341,#1736);
#882=LINE('',#16345,#1737);
#883=LINE('',#16349,#1738);
#884=LINE('',#16353,#1739);
#885=LINE('',#16357,#1740);
#886=LINE('',#16363,#1741);
#887=LINE('',#16369,#1742);
#888=LINE('',#16375,#1743);
#889=LINE('',#16381,#1744);
#890=LINE('',#16387,#1745);
#891=LINE('',#16393,#1746);
#892=LINE('',#16399,#1747);
#893=LINE('',#16405,#1748);
#894=LINE('',#16411,#1749);
#895=LINE('',#16417,#1750);
#896=LINE('',#16423,#1751);
#897=LINE('',#16427,#1752);
#898=LINE('',#16429,#1753);
#899=LINE('',#16430,#1754);
#900=LINE('',#16432,#1755);
#901=LINE('',#16435,#1756);
#902=LINE('',#16436,#1757);
#903=LINE('',#16439,#1758);
#904=LINE('',#16440,#1759);
#905=LINE('',#16443,#1760);
#906=LINE('',#16444,#1761);
#907=LINE('',#16447,#1762);
#908=LINE('',#16448,#1763);
#909=LINE('',#16450,#1764);
#910=LINE('',#16456,#1765);
#911=LINE('',#16458,#1766);
#912=LINE('',#16460,#1767);
#913=LINE('',#16462,#1768);
#914=LINE('',#16464,#1769);
#915=LINE('',#16465,#1770);
#916=LINE('',#16470,#1771);
#917=LINE('',#16472,#1772);
#918=LINE('',#16473,#1773);
#919=LINE('',#16476,#1774);
#920=LINE('',#16477,#1775);
#921=LINE('',#16480,#1776);
#922=LINE('',#16481,#1777);
#923=LINE('',#16484,#1778);
#924=LINE('',#16485,#1779);
#925=LINE('',#16488,#1780);
#926=LINE('',#16489,#1781);
#927=LINE('',#16491,#1782);
#928=LINE('',#16496,#1783);
#929=LINE('',#16502,#1784);
#930=LINE('',#16504,#1785);
#931=LINE('',#16506,#1786);
#932=LINE('',#16507,#1787);
#933=LINE('',#16512,#1788);
#934=LINE('',#16516,#1789);
#935=LINE('',#16518,#1790);
#936=LINE('',#16519,#1791);
#937=LINE('',#16523,#1792);
#938=LINE('',#16525,#1793);
#939=LINE('',#16527,#1794);
#940=LINE('',#16528,#1795);
#941=LINE('',#16533,#1796);
#942=LINE('',#16537,#1797);
#943=LINE('',#16539,#1798);
#944=LINE('',#16540,#1799);
#945=LINE('',#16545,#1800);
#946=LINE('',#16552,#1801);
#947=LINE('',#16555,#1802);
#948=LINE('',#16557,#1803);
#949=LINE('',#16558,#1804);
#950=LINE('',#16562,#1805);
#951=LINE('',#16564,#1806);
#952=LINE('',#16566,#1807);
#953=LINE('',#16567,#1808);
#954=LINE('',#16573,#1809);
#955=LINE('',#16576,#1810);
#956=LINE('',#16578,#1811);
#957=LINE('',#16579,#1812);
#958=LINE('',#16583,#1813);
#959=LINE('',#16585,#1814);
#960=LINE('',#16587,#1815);
#961=LINE('',#16588,#1816);
#962=LINE('',#16594,#1817);
#963=LINE('',#16597,#1818);
#964=LINE('',#16599,#1819);
#965=LINE('',#16600,#1820);
#966=LINE('',#16606,#1821);
#967=LINE('',#16608,#1822);
#968=LINE('',#16609,#1823);
#969=LINE('',#16615,#1824);
#970=LINE('',#16617,#1825);
#971=LINE('',#16618,#1826);
#972=LINE('',#16621,#1827);
#973=LINE('',#16623,#1828);
#974=LINE('',#16624,#1829);
#975=LINE('',#16626,#1830);
#976=LINE('',#16627,#1831);
#977=LINE('',#16632,#1832);
#978=LINE('',#16636,#1833);
#979=LINE('',#16638,#1834);
#980=LINE('',#16639,#1835);
#981=LINE('',#16644,#1836);
#982=LINE('',#16648,#1837);
#983=LINE('',#16650,#1838);
#984=LINE('',#16651,#1839);
#985=LINE('',#16654,#1840);
#986=LINE('',#16656,#1841);
#987=LINE('',#16657,#1842);
#988=LINE('',#16660,#1843);
#989=LINE('',#16662,#1844);
#990=LINE('',#16663,#1845);
#991=LINE('',#16668,#1846);
#992=LINE('',#16672,#1847);
#993=LINE('',#16674,#1848);
#994=LINE('',#16675,#1849);
#995=LINE('',#16680,#1850);
#996=LINE('',#16684,#1851);
#997=LINE('',#16686,#1852);
#998=LINE('',#16687,#1853);
#999=LINE('',#16693,#1854);
#1000=LINE('',#16696,#1855);
#1001=LINE('',#16698,#1856);
#1002=LINE('',#16699,#1857);
#1003=LINE('',#16705,#1858);
#1004=LINE('',#16708,#1859);
#1005=LINE('',#16710,#1860);
#1006=LINE('',#16711,#1861);
#1007=LINE('',#16714,#1862);
#1008=LINE('',#16716,#1863);
#1009=LINE('',#16717,#1864);
#1010=LINE('',#16720,#1865);
#1011=LINE('',#16722,#1866);
#1012=LINE('',#16723,#1867);
#1013=LINE('',#16729,#1868);
#1014=LINE('',#16732,#1869);
#1015=LINE('',#16734,#1870);
#1016=LINE('',#16735,#1871);
#1017=LINE('',#16746,#1872);
#1018=LINE('',#16752,#1873);
#1019=LINE('',#16758,#1874);
#1020=LINE('',#16764,#1875);
#1021=LINE('',#16770,#1876);
#1022=LINE('',#16775,#1877);
#1023=LINE('',#16777,#1878);
#1024=LINE('',#16779,#1879);
#1025=LINE('',#16780,#1880);
#1026=LINE('',#16786,#1881);
#1027=LINE('',#16789,#1882);
#1028=LINE('',#16791,#1883);
#1029=LINE('',#16792,#1884);
#1030=LINE('',#16799,#1885);
#1031=LINE('',#16801,#1886);
#1032=LINE('',#16803,#1887);
#1033=LINE('',#16804,#1888);
#1034=LINE('',#16810,#1889);
#1035=LINE('',#16813,#1890);
#1036=LINE('',#16815,#1891);
#1037=LINE('',#16816,#1892);
#1038=LINE('',#16824,#1893);
#1039=LINE('',#16830,#1894);
#1040=LINE('',#16836,#1895);
#1041=LINE('',#16842,#1896);
#1042=LINE('',#16848,#1897);
#1043=LINE('',#16853,#1898);
#1044=LINE('',#16855,#1899);
#1045=LINE('',#16857,#1900);
#1046=LINE('',#16858,#1901);
#1047=LINE('',#16864,#1902);
#1048=LINE('',#16867,#1903);
#1049=LINE('',#16869,#1904);
#1050=LINE('',#16870,#1905);
#1051=LINE('',#16877,#1906);
#1052=LINE('',#16879,#1907);
#1053=LINE('',#16881,#1908);
#1054=LINE('',#16882,#1909);
#1055=LINE('',#16888,#1910);
#1056=LINE('',#16891,#1911);
#1057=LINE('',#16893,#1912);
#1058=LINE('',#16894,#1913);
#1059=LINE('',#16902,#1914);
#1060=LINE('',#16908,#1915);
#1061=LINE('',#16914,#1916);
#1062=LINE('',#16920,#1917);
#1063=LINE('',#16926,#1918);
#1064=LINE('',#16931,#1919);
#1065=LINE('',#16933,#1920);
#1066=LINE('',#16935,#1921);
#1067=LINE('',#16936,#1922);
#1068=LINE('',#16942,#1923);
#1069=LINE('',#16945,#1924);
#1070=LINE('',#16947,#1925);
#1071=LINE('',#16948,#1926);
#1072=LINE('',#16955,#1927);
#1073=LINE('',#16957,#1928);
#1074=LINE('',#16959,#1929);
#1075=LINE('',#16960,#1930);
#1076=LINE('',#16966,#1931);
#1077=LINE('',#16969,#1932);
#1078=LINE('',#16971,#1933);
#1079=LINE('',#16972,#1934);
#1080=LINE('',#16980,#1935);
#1081=LINE('',#16986,#1936);
#1082=LINE('',#16992,#1937);
#1083=LINE('',#16998,#1938);
#1084=LINE('',#17004,#1939);
#1085=LINE('',#17009,#1940);
#1086=LINE('',#17011,#1941);
#1087=LINE('',#17013,#1942);
#1088=LINE('',#17014,#1943);
#1089=LINE('',#17020,#1944);
#1090=LINE('',#17023,#1945);
#1091=LINE('',#17025,#1946);
#1092=LINE('',#17026,#1947);
#1093=LINE('',#17033,#1948);
#1094=LINE('',#17035,#1949);
#1095=LINE('',#17037,#1950);
#1096=LINE('',#17038,#1951);
#1097=LINE('',#17044,#1952);
#1098=LINE('',#17047,#1953);
#1099=LINE('',#17049,#1954);
#1100=LINE('',#17050,#1955);
#1101=LINE('',#17058,#1956);
#1102=LINE('',#17064,#1957);
#1103=LINE('',#17070,#1958);
#1104=LINE('',#17076,#1959);
#1105=LINE('',#17082,#1960);
#1106=LINE('',#17087,#1961);
#1107=LINE('',#17089,#1962);
#1108=LINE('',#17091,#1963);
#1109=LINE('',#17092,#1964);
#1110=LINE('',#17098,#1965);
#1111=LINE('',#17101,#1966);
#1112=LINE('',#17103,#1967);
#1113=LINE('',#17104,#1968);
#1114=LINE('',#17111,#1969);
#1115=LINE('',#17113,#1970);
#1116=LINE('',#17115,#1971);
#1117=LINE('',#17116,#1972);
#1118=LINE('',#17122,#1973);
#1119=LINE('',#17125,#1974);
#1120=LINE('',#17127,#1975);
#1121=LINE('',#17128,#1976);
#1122=LINE('',#17136,#1977);
#1123=LINE('',#17142,#1978);
#1124=LINE('',#17148,#1979);
#1125=LINE('',#17154,#1980);
#1126=LINE('',#17160,#1981);
#1127=LINE('',#17165,#1982);
#1128=LINE('',#17167,#1983);
#1129=LINE('',#17169,#1984);
#1130=LINE('',#17170,#1985);
#1131=LINE('',#17176,#1986);
#1132=LINE('',#17179,#1987);
#1133=LINE('',#17181,#1988);
#1134=LINE('',#17182,#1989);
#1135=LINE('',#17189,#1990);
#1136=LINE('',#17191,#1991);
#1137=LINE('',#17193,#1992);
#1138=LINE('',#17194,#1993);
#1139=LINE('',#17200,#1994);
#1140=LINE('',#17203,#1995);
#1141=LINE('',#17205,#1996);
#1142=LINE('',#17206,#1997);
#1143=LINE('',#17214,#1998);
#1144=LINE('',#17220,#1999);
#1145=LINE('',#17226,#2000);
#1146=LINE('',#17232,#2001);
#1147=LINE('',#17238,#2002);
#1148=LINE('',#17243,#2003);
#1149=LINE('',#17245,#2004);
#1150=LINE('',#17247,#2005);
#1151=LINE('',#17248,#2006);
#1152=LINE('',#17254,#2007);
#1153=LINE('',#17257,#2008);
#1154=LINE('',#17259,#2009);
#1155=LINE('',#17260,#2010);
#1156=LINE('',#17267,#2011);
#1157=LINE('',#17269,#2012);
#1158=LINE('',#17271,#2013);
#1159=LINE('',#17272,#2014);
#1160=LINE('',#17278,#2015);
#1161=LINE('',#17281,#2016);
#1162=LINE('',#17283,#2017);
#1163=LINE('',#17284,#2018);
#1164=LINE('',#17292,#2019);
#1165=LINE('',#17298,#2020);
#1166=LINE('',#17304,#2021);
#1167=LINE('',#17310,#2022);
#1168=LINE('',#17316,#2023);
#1169=LINE('',#17321,#2024);
#1170=LINE('',#17323,#2025);
#1171=LINE('',#17325,#2026);
#1172=LINE('',#17326,#2027);
#1173=LINE('',#17332,#2028);
#1174=LINE('',#17335,#2029);
#1175=LINE('',#17337,#2030);
#1176=LINE('',#17338,#2031);
#1177=LINE('',#17345,#2032);
#1178=LINE('',#17347,#2033);
#1179=LINE('',#17349,#2034);
#1180=LINE('',#17350,#2035);
#1181=LINE('',#17356,#2036);
#1182=LINE('',#17359,#2037);
#1183=LINE('',#17361,#2038);
#1184=LINE('',#17362,#2039);
#1185=LINE('',#17370,#2040);
#1186=LINE('',#17376,#2041);
#1187=LINE('',#17382,#2042);
#1188=LINE('',#17388,#2043);
#1189=LINE('',#17394,#2044);
#1190=LINE('',#17399,#2045);
#1191=LINE('',#17401,#2046);
#1192=LINE('',#17403,#2047);
#1193=LINE('',#17404,#2048);
#1194=LINE('',#17410,#2049);
#1195=LINE('',#17413,#2050);
#1196=LINE('',#17415,#2051);
#1197=LINE('',#17416,#2052);
#1198=LINE('',#17423,#2053);
#1199=LINE('',#17425,#2054);
#1200=LINE('',#17427,#2055);
#1201=LINE('',#17428,#2056);
#1202=LINE('',#17434,#2057);
#1203=LINE('',#17437,#2058);
#1204=LINE('',#17439,#2059);
#1205=LINE('',#17440,#2060);
#1206=LINE('',#17448,#2061);
#1207=LINE('',#17454,#2062);
#1208=LINE('',#17459,#2063);
#1209=LINE('',#17461,#2064);
#1210=LINE('',#17463,#2065);
#1211=LINE('',#17464,#2066);
#1212=LINE('',#17470,#2067);
#1213=LINE('',#17473,#2068);
#1214=LINE('',#17475,#2069);
#1215=LINE('',#17476,#2070);
#1216=LINE('',#17483,#2071);
#1217=LINE('',#17485,#2072);
#1218=LINE('',#17487,#2073);
#1219=LINE('',#17488,#2074);
#1220=LINE('',#17494,#2075);
#1221=LINE('',#17497,#2076);
#1222=LINE('',#17499,#2077);
#1223=LINE('',#17500,#2078);
#1224=LINE('',#17508,#2079);
#1225=LINE('',#17514,#2080);
#1226=LINE('',#17520,#2081);
#1227=LINE('',#17527,#2082);
#1228=LINE('',#17530,#2083);
#1229=LINE('',#17533,#2084);
#1230=LINE('',#17535,#2085);
#1231=LINE('',#17536,#2086);
#1232=LINE('',#17541,#2087);
#1233=LINE('',#17545,#2088);
#1234=LINE('',#17547,#2089);
#1235=LINE('',#17548,#2090);
#1236=LINE('',#17648,#2091);
#1237=LINE('',#17651,#2092);
#1238=LINE('',#17654,#2093);
#1239=LINE('',#17656,#2094);
#1240=LINE('',#17657,#2095);
#1241=LINE('',#17660,#2096);
#1242=LINE('',#17661,#2097);
#1243=LINE('',#17663,#2098);
#1244=LINE('',#17665,#2099);
#1245=LINE('',#17667,#2100);
#1246=LINE('',#17672,#2101);
#1247=LINE('',#17676,#2102);
#1248=LINE('',#17680,#2103);
#1249=LINE('',#17684,#2104);
#1250=LINE('',#17688,#2105);
#1251=LINE('',#17692,#2106);
#1252=LINE('',#17696,#2107);
#1253=LINE('',#17700,#2108);
#1254=LINE('',#17704,#2109);
#1255=LINE('',#17708,#2110);
#1256=LINE('',#17712,#2111);
#1257=LINE('',#17716,#2112);
#1258=LINE('',#17720,#2113);
#1259=LINE('',#17724,#2114);
#1260=LINE('',#17728,#2115);
#1261=LINE('',#17732,#2116);
#1262=LINE('',#17736,#2117);
#1263=LINE('',#17740,#2118);
#1264=LINE('',#17744,#2119);
#1265=LINE('',#17748,#2120);
#1266=LINE('',#17752,#2121);
#1267=LINE('',#17756,#2122);
#1268=LINE('',#17760,#2123);
#1269=LINE('',#17764,#2124);
#1270=LINE('',#17768,#2125);
#1271=LINE('',#17772,#2126);
#1272=LINE('',#17776,#2127);
#1273=LINE('',#17780,#2128);
#1274=LINE('',#17784,#2129);
#1275=LINE('',#17788,#2130);
#1276=LINE('',#17792,#2131);
#1277=LINE('',#17796,#2132);
#1278=LINE('',#17800,#2133);
#1279=LINE('',#17804,#2134);
#1280=LINE('',#17808,#2135);
#1281=LINE('',#17812,#2136);
#1282=LINE('',#17816,#2137);
#1283=LINE('',#17820,#2138);
#1284=LINE('',#17824,#2139);
#1285=LINE('',#17828,#2140);
#1286=LINE('',#17832,#2141);
#1287=LINE('',#17836,#2142);
#1288=LINE('',#17840,#2143);
#1289=LINE('',#17844,#2144);
#1290=LINE('',#17848,#2145);
#1291=LINE('',#17852,#2146);
#1292=LINE('',#17856,#2147);
#1293=LINE('',#17860,#2148);
#1294=LINE('',#17863,#2149);
#1295=LINE('',#17864,#2150);
#1296=LINE('',#17866,#2151);
#1297=LINE('',#17871,#2152);
#1298=LINE('',#17877,#2153);
#1299=LINE('',#17883,#2154);
#1300=LINE('',#17889,#2155);
#1301=LINE('',#17895,#2156);
#1302=LINE('',#17901,#2157);
#1303=LINE('',#17907,#2158);
#1304=LINE('',#17913,#2159);
#1305=LINE('',#17919,#2160);
#1306=LINE('',#17925,#2161);
#1307=LINE('',#17931,#2162);
#1308=LINE('',#17937,#2163);
#1309=LINE('',#17943,#2164);
#1310=LINE('',#17949,#2165);
#1311=LINE('',#17955,#2166);
#1312=LINE('',#17961,#2167);
#1313=LINE('',#17967,#2168);
#1314=LINE('',#17973,#2169);
#1315=LINE('',#17979,#2170);
#1316=LINE('',#17985,#2171);
#1317=LINE('',#17991,#2172);
#1318=LINE('',#17997,#2173);
#1319=LINE('',#18003,#2174);
#1320=LINE('',#18009,#2175);
#1321=LINE('',#18015,#2176);
#1322=LINE('',#18021,#2177);
#1323=LINE('',#18027,#2178);
#1324=LINE('',#18033,#2179);
#1325=LINE('',#18039,#2180);
#1326=LINE('',#18045,#2181);
#1327=LINE('',#18051,#2182);
#1328=LINE('',#18057,#2183);
#1329=LINE('',#18063,#2184);
#1330=LINE('',#18069,#2185);
#1331=LINE('',#18075,#2186);
#1332=LINE('',#18081,#2187);
#1333=LINE('',#18087,#2188);
#1334=LINE('',#18093,#2189);
#1335=LINE('',#18099,#2190);
#1336=LINE('',#18105,#2191);
#1337=LINE('',#18111,#2192);
#1338=LINE('',#18117,#2193);
#1339=LINE('',#18123,#2194);
#1340=LINE('',#18129,#2195);
#1341=LINE('',#18135,#2196);
#1342=LINE('',#18141,#2197);
#1343=LINE('',#18147,#2198);
#1344=LINE('',#18151,#2199);
#1345=LINE('',#18153,#2200);
#1346=LINE('',#18154,#2201);
#1347=LINE('',#18156,#2202);
#1348=LINE('',#18157,#2203);
#1349=LINE('',#18165,#2204);
#1350=LINE('',#18171,#2205);
#1351=LINE('',#18177,#2206);
#1352=LINE('',#18184,#2207);
#1353=LINE('',#18187,#2208);
#1354=LINE('',#18190,#2209);
#1355=LINE('',#18192,#2210);
#1356=LINE('',#18194,#2211);
#1357=LINE('',#18196,#2212);
#1358=LINE('',#18198,#2213);
#1359=LINE('',#18200,#2214);
#1360=LINE('',#18201,#2215);
#1361=LINE('',#18229,#2216);
#1362=LINE('',#18232,#2217);
#1363=LINE('',#18235,#2218);
#1364=LINE('',#18237,#2219);
#1365=LINE('',#18239,#2220);
#1366=LINE('',#18241,#2221);
#1367=LINE('',#18243,#2222);
#1368=LINE('',#18245,#2223);
#1369=LINE('',#18246,#2224);
#1370=LINE('',#18270,#2225);
#1371=LINE('',#18272,#2226);
#1372=LINE('',#18274,#2227);
#1373=LINE('',#18276,#2228);
#1374=LINE('',#18278,#2229);
#1375=LINE('',#18280,#2230);
#1376=LINE('',#18282,#2231);
#1377=LINE('',#18284,#2232);
#1378=LINE('',#18286,#2233);
#1379=LINE('',#18288,#2234);
#1380=LINE('',#18290,#2235);
#1381=LINE('',#18292,#2236);
#1382=LINE('',#18293,#2237);
#1383=LINE('',#18295,#2238);
#1384=LINE('',#18296,#2239);
#1385=LINE('',#18298,#2240);
#1386=LINE('',#18300,#2241);
#1387=LINE('',#18305,#2242);
#1388=LINE('',#18307,#2243);
#1389=LINE('',#18309,#2244);
#1390=LINE('',#18311,#2245);
#1391=LINE('',#18313,#2246);
#1392=LINE('',#18315,#2247);
#1393=LINE('',#18317,#2248);
#1394=LINE('',#18318,#2249);
#1395=LINE('',#18344,#2250);
#1396=LINE('',#18348,#2251);
#1397=LINE('',#18352,#2252);
#1398=LINE('',#18356,#2253);
#1399=LINE('',#18360,#2254);
#1400=LINE('',#18364,#2255);
#1401=LINE('',#18368,#2256);
#1402=LINE('',#18372,#2257);
#1403=LINE('',#18376,#2258);
#1404=LINE('',#18380,#2259);
#1405=LINE('',#18384,#2260);
#1406=LINE('',#18387,#2261);
#1407=LINE('',#18389,#2262);
#1408=LINE('',#18390,#2263);
#1409=LINE('',#18393,#2264);
#1410=LINE('',#18395,#2265);
#1411=LINE('',#18396,#2266);
#1412=LINE('',#18399,#2267);
#1413=LINE('',#18400,#2268);
#1414=LINE('',#18403,#2269);
#1415=LINE('',#18404,#2270);
#1416=LINE('',#18406,#2271);
#1417=LINE('',#18410,#2272);
#1418=LINE('',#18411,#2273);
#1419=LINE('',#18412,#2274);
#1420=LINE('',#18415,#2275);
#1421=LINE('',#18417,#2276);
#1422=LINE('',#18418,#2277);
#1423=LINE('',#18420,#2278);
#1424=LINE('',#18421,#2279);
#1425=LINE('',#18424,#2280);
#1426=LINE('',#18425,#2281);
#1427=LINE('',#18428,#2282);
#1428=LINE('',#18429,#2283);
#1429=LINE('',#18431,#2284);
#1430=LINE('',#18438,#2285);
#1431=LINE('',#18443,#2286);
#1432=LINE('',#18445,#2287);
#1433=LINE('',#18447,#2288);
#1434=LINE('',#18448,#2289);
#1435=LINE('',#18451,#2290);
#1436=LINE('',#18453,#2291);
#1437=LINE('',#18454,#2292);
#1438=LINE('',#18457,#2293);
#1439=LINE('',#18459,#2294);
#1440=LINE('',#18460,#2295);
#1441=LINE('',#18463,#2296);
#1442=LINE('',#18465,#2297);
#1443=LINE('',#18466,#2298);
#1444=LINE('',#18469,#2299);
#1445=LINE('',#18471,#2300);
#1446=LINE('',#18472,#2301);
#1447=LINE('',#18474,#2302);
#1448=LINE('',#18475,#2303);
#1449=LINE('',#18483,#2304);
#1450=LINE('',#18489,#2305);
#1451=LINE('',#18495,#2306);
#1452=LINE('',#18502,#2307);
#1453=LINE('',#18505,#2308);
#1454=LINE('',#18508,#2309);
#1455=LINE('',#18510,#2310);
#1456=LINE('',#18512,#2311);
#1457=LINE('',#18514,#2312);
#1458=LINE('',#18516,#2313);
#1459=LINE('',#18518,#2314);
#1460=LINE('',#18519,#2315);
#1461=LINE('',#18547,#2316);
#1462=LINE('',#18550,#2317);
#1463=LINE('',#18553,#2318);
#1464=LINE('',#18555,#2319);
#1465=LINE('',#18557,#2320);
#1466=LINE('',#18559,#2321);
#1467=LINE('',#18561,#2322);
#1468=LINE('',#18563,#2323);
#1469=LINE('',#18564,#2324);
#1470=LINE('',#18588,#2325);
#1471=LINE('',#18590,#2326);
#1472=LINE('',#18592,#2327);
#1473=LINE('',#18594,#2328);
#1474=LINE('',#18596,#2329);
#1475=LINE('',#18598,#2330);
#1476=LINE('',#18600,#2331);
#1477=LINE('',#18602,#2332);
#1478=LINE('',#18604,#2333);
#1479=LINE('',#18606,#2334);
#1480=LINE('',#18608,#2335);
#1481=LINE('',#18610,#2336);
#1482=LINE('',#18611,#2337);
#1483=LINE('',#18613,#2338);
#1484=LINE('',#18614,#2339);
#1485=LINE('',#18616,#2340);
#1486=LINE('',#18618,#2341);
#1487=LINE('',#18623,#2342);
#1488=LINE('',#18625,#2343);
#1489=LINE('',#18627,#2344);
#1490=LINE('',#18629,#2345);
#1491=LINE('',#18631,#2346);
#1492=LINE('',#18633,#2347);
#1493=LINE('',#18635,#2348);
#1494=LINE('',#18636,#2349);
#1495=LINE('',#18662,#2350);
#1496=LINE('',#18666,#2351);
#1497=LINE('',#18670,#2352);
#1498=LINE('',#18674,#2353);
#1499=LINE('',#18678,#2354);
#1500=LINE('',#18682,#2355);
#1501=LINE('',#18686,#2356);
#1502=LINE('',#18690,#2357);
#1503=LINE('',#18694,#2358);
#1504=LINE('',#18698,#2359);
#1505=LINE('',#18702,#2360);
#1506=LINE('',#18705,#2361);
#1507=LINE('',#18707,#2362);
#1508=LINE('',#18708,#2363);
#1509=LINE('',#18711,#2364);
#1510=LINE('',#18713,#2365);
#1511=LINE('',#18714,#2366);
#1512=LINE('',#18717,#2367);
#1513=LINE('',#18718,#2368);
#1514=LINE('',#18721,#2369);
#1515=LINE('',#18722,#2370);
#1516=LINE('',#18724,#2371);
#1517=LINE('',#18728,#2372);
#1518=LINE('',#18729,#2373);
#1519=LINE('',#18730,#2374);
#1520=LINE('',#18733,#2375);
#1521=LINE('',#18735,#2376);
#1522=LINE('',#18736,#2377);
#1523=LINE('',#18738,#2378);
#1524=LINE('',#18739,#2379);
#1525=LINE('',#18742,#2380);
#1526=LINE('',#18743,#2381);
#1527=LINE('',#18746,#2382);
#1528=LINE('',#18747,#2383);
#1529=LINE('',#18749,#2384);
#1530=LINE('',#18755,#2385);
#1531=LINE('',#18757,#2386);
#1532=LINE('',#18759,#2387);
#1533=LINE('',#18761,#2388);
#1534=LINE('',#18763,#2389);
#1535=LINE('',#18764,#2390);
#1536=LINE('',#18769,#2391);
#1537=LINE('',#18771,#2392);
#1538=LINE('',#18772,#2393);
#1539=LINE('',#18775,#2394);
#1540=LINE('',#18776,#2395);
#1541=LINE('',#18779,#2396);
#1542=LINE('',#18780,#2397);
#1543=LINE('',#18783,#2398);
#1544=LINE('',#18784,#2399);
#1545=LINE('',#18787,#2400);
#1546=LINE('',#18788,#2401);
#1547=LINE('',#18790,#2402);
#1548=LINE('',#18795,#2403);
#1549=LINE('',#18802,#2404);
#1550=LINE('',#18807,#2405);
#1551=LINE('',#18809,#2406);
#1552=LINE('',#18811,#2407);
#1553=LINE('',#18812,#2408);
#1554=LINE('',#18815,#2409);
#1555=LINE('',#18817,#2410);
#1556=LINE('',#18818,#2411);
#1557=LINE('',#18821,#2412);
#1558=LINE('',#18823,#2413);
#1559=LINE('',#18824,#2414);
#1560=LINE('',#18827,#2415);
#1561=LINE('',#18829,#2416);
#1562=LINE('',#18830,#2417);
#1563=LINE('',#18833,#2418);
#1564=LINE('',#18835,#2419);
#1565=LINE('',#18836,#2420);
#1566=LINE('',#18838,#2421);
#1567=LINE('',#18839,#2422);
#1568=LINE('',#18847,#2423);
#1569=LINE('',#18852,#2424);
#1570=LINE('',#18854,#2425);
#1571=LINE('',#18856,#2426);
#1572=LINE('',#18857,#2427);
#1573=LINE('',#18860,#2428);
#1574=LINE('',#18862,#2429);
#1575=LINE('',#18863,#2430);
#1576=LINE('',#18866,#2431);
#1577=LINE('',#18868,#2432);
#1578=LINE('',#18869,#2433);
#1579=LINE('',#18872,#2434);
#1580=LINE('',#18874,#2435);
#1581=LINE('',#18875,#2436);
#1582=LINE('',#18878,#2437);
#1583=LINE('',#18880,#2438);
#1584=LINE('',#18881,#2439);
#1585=LINE('',#18883,#2440);
#1586=LINE('',#18884,#2441);
#1587=LINE('',#18891,#2442);
#1588=LINE('',#18893,#2443);
#1589=LINE('',#18895,#2444);
#1590=LINE('',#18896,#2445);
#1591=LINE('',#18901,#2446);
#1592=LINE('',#18905,#2447);
#1593=LINE('',#18907,#2448);
#1594=LINE('',#18908,#2449);
#1595=LINE('',#18912,#2450);
#1596=LINE('',#18914,#2451);
#1597=LINE('',#18916,#2452);
#1598=LINE('',#18917,#2453);
#1599=LINE('',#18922,#2454);
#1600=LINE('',#18926,#2455);
#1601=LINE('',#18928,#2456);
#1602=LINE('',#18929,#2457);
#1603=LINE('',#18934,#2458);
#1604=LINE('',#18941,#2459);
#1605=LINE('',#18944,#2460);
#1606=LINE('',#18946,#2461);
#1607=LINE('',#18947,#2462);
#1608=LINE('',#18951,#2463);
#1609=LINE('',#18953,#2464);
#1610=LINE('',#18955,#2465);
#1611=LINE('',#18956,#2466);
#1612=LINE('',#18962,#2467);
#1613=LINE('',#18965,#2468);
#1614=LINE('',#18967,#2469);
#1615=LINE('',#18968,#2470);
#1616=LINE('',#18972,#2471);
#1617=LINE('',#18974,#2472);
#1618=LINE('',#18976,#2473);
#1619=LINE('',#18977,#2474);
#1620=LINE('',#18983,#2475);
#1621=LINE('',#18986,#2476);
#1622=LINE('',#18988,#2477);
#1623=LINE('',#18989,#2478);
#1624=LINE('',#18995,#2479);
#1625=LINE('',#18997,#2480);
#1626=LINE('',#18998,#2481);
#1627=LINE('',#19004,#2482);
#1628=LINE('',#19006,#2483);
#1629=LINE('',#19007,#2484);
#1630=LINE('',#19010,#2485);
#1631=LINE('',#19012,#2486);
#1632=LINE('',#19013,#2487);
#1633=LINE('',#19015,#2488);
#1634=LINE('',#19016,#2489);
#1635=LINE('',#19021,#2490);
#1636=LINE('',#19025,#2491);
#1637=LINE('',#19027,#2492);
#1638=LINE('',#19028,#2493);
#1639=LINE('',#19033,#2494);
#1640=LINE('',#19037,#2495);
#1641=LINE('',#19039,#2496);
#1642=LINE('',#19040,#2497);
#1643=LINE('',#19043,#2498);
#1644=LINE('',#19045,#2499);
#1645=LINE('',#19046,#2500);
#1646=LINE('',#19049,#2501);
#1647=LINE('',#19051,#2502);
#1648=LINE('',#19052,#2503);
#1649=LINE('',#19057,#2504);
#1650=LINE('',#19061,#2505);
#1651=LINE('',#19063,#2506);
#1652=LINE('',#19064,#2507);
#1653=LINE('',#19069,#2508);
#1654=LINE('',#19073,#2509);
#1655=LINE('',#19075,#2510);
#1656=LINE('',#19076,#2511);
#1657=LINE('',#19082,#2512);
#1658=LINE('',#19085,#2513);
#1659=LINE('',#19087,#2514);
#1660=LINE('',#19088,#2515);
#1661=LINE('',#19094,#2516);
#1662=LINE('',#19097,#2517);
#1663=LINE('',#19099,#2518);
#1664=LINE('',#19100,#2519);
#1665=LINE('',#19103,#2520);
#1666=LINE('',#19105,#2521);
#1667=LINE('',#19106,#2522);
#1668=LINE('',#19109,#2523);
#1669=LINE('',#19111,#2524);
#1670=LINE('',#19112,#2525);
#1671=LINE('',#19118,#2526);
#1672=LINE('',#19121,#2527);
#1673=LINE('',#19123,#2528);
#1674=LINE('',#19124,#2529);
#1675=LINE('',#19135,#2530);
#1676=LINE('',#19140,#2531);
#1677=LINE('',#19142,#2532);
#1678=LINE('',#19144,#2533);
#1679=LINE('',#19145,#2534);
#1680=LINE('',#19148,#2535);
#1681=LINE('',#19150,#2536);
#1682=LINE('',#19151,#2537);
#1683=LINE('',#19154,#2538);
#1684=LINE('',#19156,#2539);
#1685=LINE('',#19157,#2540);
#1686=LINE('',#19160,#2541);
#1687=LINE('',#19162,#2542);
#1688=LINE('',#19163,#2543);
#1689=LINE('',#19166,#2544);
#1690=LINE('',#19168,#2545);
#1691=LINE('',#19169,#2546);
#1692=LINE('',#19171,#2547);
#1693=LINE('',#19172,#2548);
#1694=VECTOR('',#12744,21.2480593298244);
#1695=VECTOR('',#12771,21.2480593298244);
#1696=VECTOR('',#12784,6.);
#1697=VECTOR('',#12799,21.2480593298244);
#1698=VECTOR('',#12820,20.7480593298244);
#1699=VECTOR('',#12841,20.7480593298244);
#1700=VECTOR('',#12844,16.7480593298244);
#1701=VECTOR('',#12855,20.7480593298244);
#1702=VECTOR('',#12862,15.7480593298244);
#1703=VECTOR('',#12869,15.7480593298244);
#1704=VECTOR('',#12872,16.7480593298244);
#1705=VECTOR('',#12881,6.);
#1706=VECTOR('',#12890,10.);
#1707=VECTOR('',#12893,10.);
#1708=VECTOR('',#12896,10.);
#1709=VECTOR('',#12897,10.);
#1710=VECTOR('',#12898,10.);
#1711=VECTOR('',#12923,10.);
#1712=VECTOR('',#12924,10.);
#1713=VECTOR('',#12925,10.);
#1714=VECTOR('',#12926,10.);
#1715=VECTOR('',#12927,10.);
#1716=VECTOR('',#12928,10.);
#1717=VECTOR('',#12929,10.);
#1718=VECTOR('',#12936,10.);
#1719=VECTOR('',#12941,2.5);
#1720=VECTOR('',#12948,2.5);
#1721=VECTOR('',#12955,2.5);
#1722=VECTOR('',#12962,7.5);
#1723=VECTOR('',#12969,2.5);
#1724=VECTOR('',#12976,2.5);
#1725=VECTOR('',#12983,2.5);
#1726=VECTOR('',#12990,2.5);
#1727=VECTOR('',#12997,2.5);
#1728=VECTOR('',#13004,2.5);
#1729=VECTOR('',#13011,2.5);
#1730=VECTOR('',#13016,2.5);
#1731=VECTOR('',#13021,2.5);
#1732=VECTOR('',#13026,2.5);
#1733=VECTOR('',#13031,2.5);
#1734=VECTOR('',#13036,2.5);
#1735=VECTOR('',#13041,2.5);
#1736=VECTOR('',#13046,2.5);
#1737=VECTOR('',#13051,7.5);
#1738=VECTOR('',#13056,2.5);
#1739=VECTOR('',#13061,2.5);
#1740=VECTOR('',#13066,2.5);
#1741=VECTOR('',#13073,2.5);
#1742=VECTOR('',#13080,2.5);
#1743=VECTOR('',#13087,2.5);
#1744=VECTOR('',#13094,7.5);
#1745=VECTOR('',#13101,2.5);
#1746=VECTOR('',#13108,2.5);
#1747=VECTOR('',#13115,2.5);
#1748=VECTOR('',#13122,2.5);
#1749=VECTOR('',#13129,2.5);
#1750=VECTOR('',#13136,2.5);
#1751=VECTOR('',#13143,2.5);
#1752=VECTOR('',#13148,10.);
#1753=VECTOR('',#13149,10.);
#1754=VECTOR('',#13150,10.);
#1755=VECTOR('',#13153,10.);
#1756=VECTOR('',#13156,10.);
#1757=VECTOR('',#13157,10.);
#1758=VECTOR('',#13160,10.);
#1759=VECTOR('',#13161,10.);
#1760=VECTOR('',#13164,10.);
#1761=VECTOR('',#13165,10.);
#1762=VECTOR('',#13168,10.);
#1763=VECTOR('',#13169,10.);
#1764=VECTOR('',#13172,10.);
#1765=VECTOR('',#13179,10.);
#1766=VECTOR('',#13180,10.);
#1767=VECTOR('',#13181,10.);
#1768=VECTOR('',#13182,10.);
#1769=VECTOR('',#13183,10.);
#1770=VECTOR('',#13184,10.);
#1771=VECTOR('',#13189,10.);
#1772=VECTOR('',#13190,10.);
#1773=VECTOR('',#13191,10.);
#1774=VECTOR('',#13194,10.);
#1775=VECTOR('',#13195,10.);
#1776=VECTOR('',#13198,10.);
#1777=VECTOR('',#13199,10.);
#1778=VECTOR('',#13202,10.);
#1779=VECTOR('',#13203,10.);
#1780=VECTOR('',#13206,10.);
#1781=VECTOR('',#13207,10.);
#1782=VECTOR('',#13210,10.);
#1783=VECTOR('',#13217,1.49999999999999);
#1784=VECTOR('',#13224,10.);
#1785=VECTOR('',#13225,10.);
#1786=VECTOR('',#13226,10.);
#1787=VECTOR('',#13227,10.);
#1788=VECTOR('',#13232,10.);
#1789=VECTOR('',#13237,10.);
#1790=VECTOR('',#13238,10.);
#1791=VECTOR('',#13239,10.);
#1792=VECTOR('',#13242,10.);
#1793=VECTOR('',#13243,10.);
#1794=VECTOR('',#13244,10.);
#1795=VECTOR('',#13245,10.);
#1796=VECTOR('',#13250,10.);
#1797=VECTOR('',#13255,10.);
#1798=VECTOR('',#13256,10.);
#1799=VECTOR('',#13257,10.);
#1800=VECTOR('',#13262,10.);
#1801=VECTOR('',#13271,10.);
#1802=VECTOR('',#13274,10.);
#1803=VECTOR('',#13275,10.);
#1804=VECTOR('',#13276,10.);
#1805=VECTOR('',#13279,10.);
#1806=VECTOR('',#13280,10.);
#1807=VECTOR('',#13281,10.);
#1808=VECTOR('',#13282,10.);
#1809=VECTOR('',#13289,10.);
#1810=VECTOR('',#13292,10.);
#1811=VECTOR('',#13293,10.);
#1812=VECTOR('',#13294,10.);
#1813=VECTOR('',#13297,10.);
#1814=VECTOR('',#13298,10.);
#1815=VECTOR('',#13299,10.);
#1816=VECTOR('',#13300,10.);
#1817=VECTOR('',#13307,10.);
#1818=VECTOR('',#13310,10.);
#1819=VECTOR('',#13311,10.);
#1820=VECTOR('',#13312,10.);
#1821=VECTOR('',#13321,10.);
#1822=VECTOR('',#13322,10.);
#1823=VECTOR('',#13323,10.);
#1824=VECTOR('',#13332,10.);
#1825=VECTOR('',#13333,10.);
#1826=VECTOR('',#13334,10.);
#1827=VECTOR('',#13337,10.);
#1828=VECTOR('',#13338,10.);
#1829=VECTOR('',#13339,10.);
#1830=VECTOR('',#13342,10.);
#1831=VECTOR('',#13343,10.);
#1832=VECTOR('',#13348,10.);
#1833=VECTOR('',#13353,10.);
#1834=VECTOR('',#13354,10.);
#1835=VECTOR('',#13355,10.);
#1836=VECTOR('',#13360,10.);
#1837=VECTOR('',#13365,10.);
#1838=VECTOR('',#13366,10.);
#1839=VECTOR('',#13367,10.);
#1840=VECTOR('',#13370,10.);
#1841=VECTOR('',#13371,10.);
#1842=VECTOR('',#13372,10.);
#1843=VECTOR('',#13375,10.);
#1844=VECTOR('',#13376,10.);
#1845=VECTOR('',#13377,10.);
#1846=VECTOR('',#13382,10.);
#1847=VECTOR('',#13387,10.);
#1848=VECTOR('',#13388,10.);
#1849=VECTOR('',#13389,10.);
#1850=VECTOR('',#13394,10.);
#1851=VECTOR('',#13399,10.);
#1852=VECTOR('',#13400,10.);
#1853=VECTOR('',#13401,10.);
#1854=VECTOR('',#13408,10.);
#1855=VECTOR('',#13411,10.);
#1856=VECTOR('',#13412,10.);
#1857=VECTOR('',#13413,10.);
#1858=VECTOR('',#13420,10.);
#1859=VECTOR('',#13423,10.);
#1860=VECTOR('',#13424,10.);
#1861=VECTOR('',#13425,10.);
#1862=VECTOR('',#13428,10.);
#1863=VECTOR('',#13429,10.);
#1864=VECTOR('',#13430,10.);
#1865=VECTOR('',#13433,10.);
#1866=VECTOR('',#13434,10.);
#1867=VECTOR('',#13435,10.);
#1868=VECTOR('',#13442,10.);
#1869=VECTOR('',#13445,10.);
#1870=VECTOR('',#13446,10.);
#1871=VECTOR('',#13447,10.);
#1872=VECTOR('',#13464,2.5);
#1873=VECTOR('',#13471,2.5);
#1874=VECTOR('',#13478,2.5);
#1875=VECTOR('',#13485,2.5);
#1876=VECTOR('',#13492,10.);
#1877=VECTOR('',#13497,10.);
#1878=VECTOR('',#13498,10.);
#1879=VECTOR('',#13499,10.);
#1880=VECTOR('',#13500,10.);
#1881=VECTOR('',#13507,10.);
#1882=VECTOR('',#13510,10.);
#1883=VECTOR('',#13511,10.);
#1884=VECTOR('',#13512,10.);
#1885=VECTOR('',#13521,10.);
#1886=VECTOR('',#13522,10.);
#1887=VECTOR('',#13523,10.);
#1888=VECTOR('',#13524,10.);
#1889=VECTOR('',#13531,10.);
#1890=VECTOR('',#13534,10.);
#1891=VECTOR('',#13535,10.);
#1892=VECTOR('',#13536,10.);
#1893=VECTOR('',#13547,2.5);
#1894=VECTOR('',#13554,2.5);
#1895=VECTOR('',#13561,2.5);
#1896=VECTOR('',#13568,2.5);
#1897=VECTOR('',#13575,10.);
#1898=VECTOR('',#13580,10.);
#1899=VECTOR('',#13581,10.);
#1900=VECTOR('',#13582,10.);
#1901=VECTOR('',#13583,10.);
#1902=VECTOR('',#13590,10.);
#1903=VECTOR('',#13593,10.);
#1904=VECTOR('',#13594,10.);
#1905=VECTOR('',#13595,10.);
#1906=VECTOR('',#13604,10.);
#1907=VECTOR('',#13605,10.);
#1908=VECTOR('',#13606,10.);
#1909=VECTOR('',#13607,10.);
#1910=VECTOR('',#13614,10.);
#1911=VECTOR('',#13617,10.);
#1912=VECTOR('',#13618,10.);
#1913=VECTOR('',#13619,10.);
#1914=VECTOR('',#13630,2.5);
#1915=VECTOR('',#13637,2.5);
#1916=VECTOR('',#13644,2.5);
#1917=VECTOR('',#13651,2.5);
#1918=VECTOR('',#13658,10.);
#1919=VECTOR('',#13663,10.);
#1920=VECTOR('',#13664,10.);
#1921=VECTOR('',#13665,10.);
#1922=VECTOR('',#13666,10.);
#1923=VECTOR('',#13673,10.);
#1924=VECTOR('',#13676,10.);
#1925=VECTOR('',#13677,10.);
#1926=VECTOR('',#13678,10.);
#1927=VECTOR('',#13687,10.);
#1928=VECTOR('',#13688,10.);
#1929=VECTOR('',#13689,10.);
#1930=VECTOR('',#13690,10.);
#1931=VECTOR('',#13697,10.);
#1932=VECTOR('',#13700,10.);
#1933=VECTOR('',#13701,10.);
#1934=VECTOR('',#13702,10.);
#1935=VECTOR('',#13713,2.5);
#1936=VECTOR('',#13720,2.5);
#1937=VECTOR('',#13727,2.5);
#1938=VECTOR('',#13734,2.5);
#1939=VECTOR('',#13741,10.);
#1940=VECTOR('',#13746,10.);
#1941=VECTOR('',#13747,10.);
#1942=VECTOR('',#13748,10.);
#1943=VECTOR('',#13749,10.);
#1944=VECTOR('',#13756,10.);
#1945=VECTOR('',#13759,10.);
#1946=VECTOR('',#13760,10.);
#1947=VECTOR('',#13761,10.);
#1948=VECTOR('',#13770,10.);
#1949=VECTOR('',#13771,10.);
#1950=VECTOR('',#13772,10.);
#1951=VECTOR('',#13773,10.);
#1952=VECTOR('',#13780,10.);
#1953=VECTOR('',#13783,10.);
#1954=VECTOR('',#13784,10.);
#1955=VECTOR('',#13785,10.);
#1956=VECTOR('',#13796,2.5);
#1957=VECTOR('',#13803,2.5);
#1958=VECTOR('',#13810,2.5);
#1959=VECTOR('',#13817,2.5);
#1960=VECTOR('',#13824,10.);
#1961=VECTOR('',#13829,10.);
#1962=VECTOR('',#13830,10.);
#1963=VECTOR('',#13831,10.);
#1964=VECTOR('',#13832,10.);
#1965=VECTOR('',#13839,10.);
#1966=VECTOR('',#13842,10.);
#1967=VECTOR('',#13843,10.);
#1968=VECTOR('',#13844,10.);
#1969=VECTOR('',#13853,10.);
#1970=VECTOR('',#13854,10.);
#1971=VECTOR('',#13855,10.);
#1972=VECTOR('',#13856,10.);
#1973=VECTOR('',#13863,10.);
#1974=VECTOR('',#13866,10.);
#1975=VECTOR('',#13867,10.);
#1976=VECTOR('',#13868,10.);
#1977=VECTOR('',#13879,2.5);
#1978=VECTOR('',#13886,2.5);
#1979=VECTOR('',#13893,2.5);
#1980=VECTOR('',#13900,2.5);
#1981=VECTOR('',#13907,10.);
#1982=VECTOR('',#13912,10.);
#1983=VECTOR('',#13913,10.);
#1984=VECTOR('',#13914,10.);
#1985=VECTOR('',#13915,10.);
#1986=VECTOR('',#13922,10.);
#1987=VECTOR('',#13925,10.);
#1988=VECTOR('',#13926,10.);
#1989=VECTOR('',#13927,10.);
#1990=VECTOR('',#13936,10.);
#1991=VECTOR('',#13937,10.);
#1992=VECTOR('',#13938,10.);
#1993=VECTOR('',#13939,10.);
#1994=VECTOR('',#13946,10.);
#1995=VECTOR('',#13949,10.);
#1996=VECTOR('',#13950,10.);
#1997=VECTOR('',#13951,10.);
#1998=VECTOR('',#13962,2.5);
#1999=VECTOR('',#13969,2.5);
#2000=VECTOR('',#13976,2.5);
#2001=VECTOR('',#13983,2.5);
#2002=VECTOR('',#13990,10.);
#2003=VECTOR('',#13995,10.);
#2004=VECTOR('',#13996,10.);
#2005=VECTOR('',#13997,10.);
#2006=VECTOR('',#13998,10.);
#2007=VECTOR('',#14005,10.);
#2008=VECTOR('',#14008,10.);
#2009=VECTOR('',#14009,10.);
#2010=VECTOR('',#14010,10.);
#2011=VECTOR('',#14019,10.);
#2012=VECTOR('',#14020,10.);
#2013=VECTOR('',#14021,10.);
#2014=VECTOR('',#14022,10.);
#2015=VECTOR('',#14029,10.);
#2016=VECTOR('',#14032,10.);
#2017=VECTOR('',#14033,10.);
#2018=VECTOR('',#14034,10.);
#2019=VECTOR('',#14045,2.5);
#2020=VECTOR('',#14052,2.5);
#2021=VECTOR('',#14059,2.5);
#2022=VECTOR('',#14066,2.5);
#2023=VECTOR('',#14073,10.);
#2024=VECTOR('',#14078,10.);
#2025=VECTOR('',#14079,10.);
#2026=VECTOR('',#14080,10.);
#2027=VECTOR('',#14081,10.);
#2028=VECTOR('',#14088,10.);
#2029=VECTOR('',#14091,10.);
#2030=VECTOR('',#14092,10.);
#2031=VECTOR('',#14093,10.);
#2032=VECTOR('',#14102,10.);
#2033=VECTOR('',#14103,10.);
#2034=VECTOR('',#14104,10.);
#2035=VECTOR('',#14105,10.);
#2036=VECTOR('',#14112,10.);
#2037=VECTOR('',#14115,10.);
#2038=VECTOR('',#14116,10.);
#2039=VECTOR('',#14117,10.);
#2040=VECTOR('',#14128,2.5);
#2041=VECTOR('',#14135,2.5);
#2042=VECTOR('',#14142,2.5);
#2043=VECTOR('',#14149,2.5);
#2044=VECTOR('',#14156,10.);
#2045=VECTOR('',#14161,10.);
#2046=VECTOR('',#14162,10.);
#2047=VECTOR('',#14163,10.);
#2048=VECTOR('',#14164,10.);
#2049=VECTOR('',#14171,10.);
#2050=VECTOR('',#14174,10.);
#2051=VECTOR('',#14175,10.);
#2052=VECTOR('',#14176,10.);
#2053=VECTOR('',#14185,10.);
#2054=VECTOR('',#14186,10.);
#2055=VECTOR('',#14187,10.);
#2056=VECTOR('',#14188,10.);
#2057=VECTOR('',#14195,10.);
#2058=VECTOR('',#14198,10.);
#2059=VECTOR('',#14199,10.);
#2060=VECTOR('',#14200,10.);
#2061=VECTOR('',#14211,2.5);
#2062=VECTOR('',#14218,2.5);
#2063=VECTOR('',#14223,10.);
#2064=VECTOR('',#14224,10.);
#2065=VECTOR('',#14225,10.);
#2066=VECTOR('',#14226,10.);
#2067=VECTOR('',#14233,10.);
#2068=VECTOR('',#14236,10.);
#2069=VECTOR('',#14237,10.);
#2070=VECTOR('',#14238,10.);
#2071=VECTOR('',#14247,10.);
#2072=VECTOR('',#14248,10.);
#2073=VECTOR('',#14249,10.);
#2074=VECTOR('',#14250,10.);
#2075=VECTOR('',#14257,10.);
#2076=VECTOR('',#14260,10.);
#2077=VECTOR('',#14261,10.);
#2078=VECTOR('',#14262,10.);
#2079=VECTOR('',#14273,10.);
#2080=VECTOR('',#14280,2.5);
#2081=VECTOR('',#14287,2.5);
#2082=VECTOR('',#14294,10.);
#2083=VECTOR('',#14297,10.);
#2084=VECTOR('',#14300,10.);
#2085=VECTOR('',#14301,10.);
#2086=VECTOR('',#14302,10.);
#2087=VECTOR('',#14307,10.);
#2088=VECTOR('',#14312,10.);
#2089=VECTOR('',#14313,10.);
#2090=VECTOR('',#14314,10.);
#2091=VECTOR('',#14413,10.);
#2092=VECTOR('',#14416,10.);
#2093=VECTOR('',#14419,10.);
#2094=VECTOR('',#14420,10.);
#2095=VECTOR('',#14421,10.);
#2096=VECTOR('',#14424,10.);
#2097=VECTOR('',#14425,10.);
#2098=VECTOR('',#14426,10.);
#2099=VECTOR('',#14427,10.);
#2100=VECTOR('',#14428,10.);
#2101=VECTOR('',#14435,10.);
#2102=VECTOR('',#14440,2.);
#2103=VECTOR('',#14445,1.99999999999999);
#2104=VECTOR('',#14450,2.00000000000003);
#2105=VECTOR('',#14455,1.99999999999999);
#2106=VECTOR('',#14460,2.00000000000003);
#2107=VECTOR('',#14465,2.);
#2108=VECTOR('',#14470,1.99999999999999);
#2109=VECTOR('',#14475,1.99999999999999);
#2110=VECTOR('',#14480,1.99999999999999);
#2111=VECTOR('',#14485,1.99999999999999);
#2112=VECTOR('',#14490,1.99999999999999);
#2113=VECTOR('',#14495,1.99999999999999);
#2114=VECTOR('',#14500,2.);
#2115=VECTOR('',#14505,1.99999999999999);
#2116=VECTOR('',#14510,1.99999999999999);
#2117=VECTOR('',#14515,1.99999999999999);
#2118=VECTOR('',#14520,1.99999999999999);
#2119=VECTOR('',#14525,2.);
#2120=VECTOR('',#14530,2.);
#2121=VECTOR('',#14535,2.00000000000003);
#2122=VECTOR('',#14540,2.);
#2123=VECTOR('',#14545,1.99999999999999);
#2124=VECTOR('',#14550,2.);
#2125=VECTOR('',#14555,1.99999999999999);
#2126=VECTOR('',#14560,1.99999999999999);
#2127=VECTOR('',#14565,1.99999999999999);
#2128=VECTOR('',#14570,1.99999999999999);
#2129=VECTOR('',#14575,1.99999999999999);
#2130=VECTOR('',#14580,1.99999999999999);
#2131=VECTOR('',#14585,1.99999999999999);
#2132=VECTOR('',#14590,2.);
#2133=VECTOR('',#14595,2.00000000000003);
#2134=VECTOR('',#14600,1.99999999999999);
#2135=VECTOR('',#14605,1.99999999999999);
#2136=VECTOR('',#14610,1.99999999999999);
#2137=VECTOR('',#14615,1.99999999999999);
#2138=VECTOR('',#14620,2.);
#2139=VECTOR('',#14625,2.00000000000003);
#2140=VECTOR('',#14630,2.00000000000003);
#2141=VECTOR('',#14635,2.00000000000003);
#2142=VECTOR('',#14640,1.99999999999999);
#2143=VECTOR('',#14645,1.99999999999999);
#2144=VECTOR('',#14650,1.99999999999999);
#2145=VECTOR('',#14655,2.00000000000003);
#2146=VECTOR('',#14660,1.99999999999999);
#2147=VECTOR('',#14665,1.99999999999999);
#2148=VECTOR('',#14670,1.99999999999999);
#2149=VECTOR('',#14673,10.);
#2150=VECTOR('',#14674,10.);
#2151=VECTOR('',#14677,10.);
#2152=VECTOR('',#14682,2.);
#2153=VECTOR('',#14689,1.99999999999999);
#2154=VECTOR('',#14696,2.00000000000003);
#2155=VECTOR('',#14703,1.99999999999999);
#2156=VECTOR('',#14710,2.00000000000003);
#2157=VECTOR('',#14717,2.);
#2158=VECTOR('',#14724,1.99999999999999);
#2159=VECTOR('',#14731,1.99999999999999);
#2160=VECTOR('',#14738,1.99999999999999);
#2161=VECTOR('',#14745,1.99999999999999);
#2162=VECTOR('',#14752,1.99999999999999);
#2163=VECTOR('',#14759,1.99999999999999);
#2164=VECTOR('',#14766,2.);
#2165=VECTOR('',#14773,1.99999999999999);
#2166=VECTOR('',#14780,1.99999999999999);
#2167=VECTOR('',#14787,1.99999999999999);
#2168=VECTOR('',#14794,1.99999999999999);
#2169=VECTOR('',#14801,2.);
#2170=VECTOR('',#14808,2.);
#2171=VECTOR('',#14815,2.00000000000003);
#2172=VECTOR('',#14822,2.);
#2173=VECTOR('',#14829,1.99999999999999);
#2174=VECTOR('',#14836,2.);
#2175=VECTOR('',#14843,1.99999999999999);
#2176=VECTOR('',#14850,1.99999999999999);
#2177=VECTOR('',#14857,1.99999999999999);
#2178=VECTOR('',#14864,1.99999999999999);
#2179=VECTOR('',#14871,1.99999999999999);
#2180=VECTOR('',#14878,1.99999999999999);
#2181=VECTOR('',#14885,1.99999999999999);
#2182=VECTOR('',#14892,2.);
#2183=VECTOR('',#14899,2.00000000000003);
#2184=VECTOR('',#14906,1.99999999999999);
#2185=VECTOR('',#14913,1.99999999999999);
#2186=VECTOR('',#14920,1.99999999999999);
#2187=VECTOR('',#14927,1.99999999999999);
#2188=VECTOR('',#14934,2.);
#2189=VECTOR('',#14941,2.00000000000003);
#2190=VECTOR('',#14948,2.00000000000003);
#2191=VECTOR('',#14955,2.00000000000003);
#2192=VECTOR('',#14962,1.99999999999999);
#2193=VECTOR('',#14969,1.99999999999999);
#2194=VECTOR('',#14976,1.99999999999999);
#2195=VECTOR('',#14983,2.00000000000003);
#2196=VECTOR('',#14990,1.99999999999999);
#2197=VECTOR('',#14997,1.99999999999999);
#2198=VECTOR('',#15004,1.99999999999999);
#2199=VECTOR('',#15009,10.);
#2200=VECTOR('',#15010,10.);
#2201=VECTOR('',#15011,10.);
#2202=VECTOR('',#15014,10.);
#2203=VECTOR('',#15015,10.);
#2204=VECTOR('',#15026,1.49999999999999);
#2205=VECTOR('',#15033,2.00000000000003);
#2206=VECTOR('',#15040,2.00000000000003);
#2207=VECTOR('',#15047,10.);
#2208=VECTOR('',#15050,10.);
#2209=VECTOR('',#15053,10.);
#2210=VECTOR('',#15054,10.);
#2211=VECTOR('',#15055,10.);
#2212=VECTOR('',#15056,10.);
#2213=VECTOR('',#15057,10.);
#2214=VECTOR('',#15058,10.);
#2215=VECTOR('',#15059,10.);
#2216=VECTOR('',#15086,4.);
#2217=VECTOR('',#15089,10.);
#2218=VECTOR('',#15092,10.);
#2219=VECTOR('',#15093,10.);
#2220=VECTOR('',#15094,10.);
#2221=VECTOR('',#15095,10.);
#2222=VECTOR('',#15096,10.);
#2223=VECTOR('',#15097,10.);
#2224=VECTOR('',#15098,10.);
#2225=VECTOR('',#15123,1.49999999999999);
#2226=VECTOR('',#15126,1.49999999999999);
#2227=VECTOR('',#15129,1.49999999999999);
#2228=VECTOR('',#15132,1.49999999999999);
#2229=VECTOR('',#15135,1.49999999999999);
#2230=VECTOR('',#15138,1.49999999999999);
#2231=VECTOR('',#15141,1.49999999999999);
#2232=VECTOR('',#15144,1.49999999999999);
#2233=VECTOR('',#15147,1.49999999999999);
#2234=VECTOR('',#15150,1.49999999999999);
#2235=VECTOR('',#15153,1.49999999999999);
#2236=VECTOR('',#15156,10.);
#2237=VECTOR('',#15157,10.);
#2238=VECTOR('',#15160,10.);
#2239=VECTOR('',#15161,10.);
#2240=VECTOR('',#15164,10.);
#2241=VECTOR('',#15167,10.);
#2242=VECTOR('',#15172,10.);
#2243=VECTOR('',#15173,10.);
#2244=VECTOR('',#15174,10.);
#2245=VECTOR('',#15175,10.);
#2246=VECTOR('',#15176,10.);
#2247=VECTOR('',#15177,10.);
#2248=VECTOR('',#15178,10.);
#2249=VECTOR('',#15179,10.);
#2250=VECTOR('',#15206,1.49999999999999);
#2251=VECTOR('',#15211,1.49999999999999);
#2252=VECTOR('',#15216,1.49999999999999);
#2253=VECTOR('',#15221,1.49999999999999);
#2254=VECTOR('',#15226,1.49999999999999);
#2255=VECTOR('',#15231,1.49999999999999);
#2256=VECTOR('',#15236,1.49999999999999);
#2257=VECTOR('',#15241,1.49999999999999);
#2258=VECTOR('',#15246,1.49999999999999);
#2259=VECTOR('',#15251,1.49999999999999);
#2260=VECTOR('',#15256,1.49999999999999);
#2261=VECTOR('',#15259,10.);
#2262=VECTOR('',#15260,10.);
#2263=VECTOR('',#15261,10.);
#2264=VECTOR('',#15264,10.);
#2265=VECTOR('',#15265,10.);
#2266=VECTOR('',#15266,10.);
#2267=VECTOR('',#15269,10.);
#2268=VECTOR('',#15270,10.);
#2269=VECTOR('',#15273,10.);
#2270=VECTOR('',#15274,10.);
#2271=VECTOR('',#15277,10.);
#2272=VECTOR('',#15280,10.);
#2273=VECTOR('',#15281,10.);
#2274=VECTOR('',#15282,10.);
#2275=VECTOR('',#15285,10.);
#2276=VECTOR('',#15286,10.);
#2277=VECTOR('',#15287,10.);
#2278=VECTOR('',#15290,10.);
#2279=VECTOR('',#15291,10.);
#2280=VECTOR('',#15294,10.);
#2281=VECTOR('',#15295,10.);
#2282=VECTOR('',#15298,10.);
#2283=VECTOR('',#15299,10.);
#2284=VECTOR('',#15302,10.);
#2285=VECTOR('',#15311,1.49999999999999);
#2286=VECTOR('',#15316,10.);
#2287=VECTOR('',#15317,10.);
#2288=VECTOR('',#15318,10.);
#2289=VECTOR('',#15319,10.);
#2290=VECTOR('',#15322,10.);
#2291=VECTOR('',#15323,10.);
#2292=VECTOR('',#15324,10.);
#2293=VECTOR('',#15327,10.);
#2294=VECTOR('',#15328,10.);
#2295=VECTOR('',#15329,10.);
#2296=VECTOR('',#15332,10.);
#2297=VECTOR('',#15333,10.);
#2298=VECTOR('',#15334,10.);
#2299=VECTOR('',#15337,10.);
#2300=VECTOR('',#15338,10.);
#2301=VECTOR('',#15339,10.);
#2302=VECTOR('',#15342,10.);
#2303=VECTOR('',#15343,10.);
#2304=VECTOR('',#15354,1.5);
#2305=VECTOR('',#15361,2.00000000000003);
#2306=VECTOR('',#15368,2.00000000000003);
#2307=VECTOR('',#15375,10.);
#2308=VECTOR('',#15378,10.);
#2309=VECTOR('',#15381,10.);
#2310=VECTOR('',#15382,10.);
#2311=VECTOR('',#15383,10.);
#2312=VECTOR('',#15384,10.);
#2313=VECTOR('',#15385,10.);
#2314=VECTOR('',#15386,10.);
#2315=VECTOR('',#15387,10.);
#2316=VECTOR('',#15414,4.);
#2317=VECTOR('',#15417,10.);
#2318=VECTOR('',#15420,10.);
#2319=VECTOR('',#15421,10.);
#2320=VECTOR('',#15422,10.);
#2321=VECTOR('',#15423,10.);
#2322=VECTOR('',#15424,10.);
#2323=VECTOR('',#15425,10.);
#2324=VECTOR('',#15426,10.);
#2325=VECTOR('',#15451,1.49999999999999);
#2326=VECTOR('',#15454,1.49999999999999);
#2327=VECTOR('',#15457,1.49999999999999);
#2328=VECTOR('',#15460,1.49999999999999);
#2329=VECTOR('',#15463,1.49999999999999);
#2330=VECTOR('',#15466,1.49999999999999);
#2331=VECTOR('',#15469,1.49999999999999);
#2332=VECTOR('',#15472,1.49999999999999);
#2333=VECTOR('',#15475,1.49999999999999);
#2334=VECTOR('',#15478,1.49999999999999);
#2335=VECTOR('',#15481,1.49999999999999);
#2336=VECTOR('',#15484,10.);
#2337=VECTOR('',#15485,10.);
#2338=VECTOR('',#15488,10.);
#2339=VECTOR('',#15489,10.);
#2340=VECTOR('',#15492,10.);
#2341=VECTOR('',#15495,10.);
#2342=VECTOR('',#15500,10.);
#2343=VECTOR('',#15501,10.);
#2344=VECTOR('',#15502,10.);
#2345=VECTOR('',#15503,10.);
#2346=VECTOR('',#15504,10.);
#2347=VECTOR('',#15505,10.);
#2348=VECTOR('',#15506,10.);
#2349=VECTOR('',#15507,10.);
#2350=VECTOR('',#15534,1.49999999999999);
#2351=VECTOR('',#15539,1.49999999999999);
#2352=VECTOR('',#15544,1.49999999999999);
#2353=VECTOR('',#15549,1.49999999999999);
#2354=VECTOR('',#15554,1.49999999999999);
#2355=VECTOR('',#15559,1.49999999999999);
#2356=VECTOR('',#15564,1.49999999999999);
#2357=VECTOR('',#15569,1.49999999999999);
#2358=VECTOR('',#15574,1.49999999999999);
#2359=VECTOR('',#15579,1.49999999999999);
#2360=VECTOR('',#15584,1.49999999999999);
#2361=VECTOR('',#15587,10.);
#2362=VECTOR('',#15588,10.);
#2363=VECTOR('',#15589,10.);
#2364=VECTOR('',#15592,10.);
#2365=VECTOR('',#15593,10.);
#2366=VECTOR('',#15594,10.);
#2367=VECTOR('',#15597,10.);
#2368=VECTOR('',#15598,10.);
#2369=VECTOR('',#15601,10.);
#2370=VECTOR('',#15602,10.);
#2371=VECTOR('',#15605,10.);
#2372=VECTOR('',#15608,10.);
#2373=VECTOR('',#15609,10.);
#2374=VECTOR('',#15610,10.);
#2375=VECTOR('',#15613,10.);
#2376=VECTOR('',#15614,10.);
#2377=VECTOR('',#15615,10.);
#2378=VECTOR('',#15618,10.);
#2379=VECTOR('',#15619,10.);
#2380=VECTOR('',#15622,10.);
#2381=VECTOR('',#15623,10.);
#2382=VECTOR('',#15626,10.);
#2383=VECTOR('',#15627,10.);
#2384=VECTOR('',#15630,10.);
#2385=VECTOR('',#15637,10.);
#2386=VECTOR('',#15638,10.);
#2387=VECTOR('',#15639,10.);
#2388=VECTOR('',#15640,10.);
#2389=VECTOR('',#15641,10.);
#2390=VECTOR('',#15642,10.);
#2391=VECTOR('',#15647,10.);
#2392=VECTOR('',#15648,10.);
#2393=VECTOR('',#15649,10.);
#2394=VECTOR('',#15652,10.);
#2395=VECTOR('',#15653,10.);
#2396=VECTOR('',#15656,10.);
#2397=VECTOR('',#15657,10.);
#2398=VECTOR('',#15660,10.);
#2399=VECTOR('',#15661,10.);
#2400=VECTOR('',#15664,10.);
#2401=VECTOR('',#15665,10.);
#2402=VECTOR('',#15668,10.);
#2403=VECTOR('',#15675,1.49999999999999);
#2404=VECTOR('',#15684,1.49999999999999);
#2405=VECTOR('',#15689,10.);
#2406=VECTOR('',#15690,10.);
#2407=VECTOR('',#15691,10.);
#2408=VECTOR('',#15692,10.);
#2409=VECTOR('',#15695,10.);
#2410=VECTOR('',#15696,10.);
#2411=VECTOR('',#15697,10.);
#2412=VECTOR('',#15700,10.);
#2413=VECTOR('',#15701,10.);
#2414=VECTOR('',#15702,10.);
#2415=VECTOR('',#15705,10.);
#2416=VECTOR('',#15706,10.);
#2417=VECTOR('',#15707,10.);
#2418=VECTOR('',#15710,10.);
#2419=VECTOR('',#15711,10.);
#2420=VECTOR('',#15712,10.);
#2421=VECTOR('',#15715,10.);
#2422=VECTOR('',#15716,10.);
#2423=VECTOR('',#15727,1.49999999999999);
#2424=VECTOR('',#15732,10.);
#2425=VECTOR('',#15733,10.);
#2426=VECTOR('',#15734,10.);
#2427=VECTOR('',#15735,10.);
#2428=VECTOR('',#15738,10.);
#2429=VECTOR('',#15739,10.);
#2430=VECTOR('',#15740,10.);
#2431=VECTOR('',#15743,10.);
#2432=VECTOR('',#15744,10.);
#2433=VECTOR('',#15745,10.);
#2434=VECTOR('',#15748,10.);
#2435=VECTOR('',#15749,10.);
#2436=VECTOR('',#15750,10.);
#2437=VECTOR('',#15753,10.);
#2438=VECTOR('',#15754,10.);
#2439=VECTOR('',#15755,10.);
#2440=VECTOR('',#15758,10.);
#2441=VECTOR('',#15759,10.);
#2442=VECTOR('',#15768,10.);
#2443=VECTOR('',#15769,10.);
#2444=VECTOR('',#15770,10.);
#2445=VECTOR('',#15771,10.);
#2446=VECTOR('',#15776,10.);
#2447=VECTOR('',#15781,10.);
#2448=VECTOR('',#15782,10.);
#2449=VECTOR('',#15783,10.);
#2450=VECTOR('',#15786,10.);
#2451=VECTOR('',#15787,10.);
#2452=VECTOR('',#15788,10.);
#2453=VECTOR('',#15789,10.);
#2454=VECTOR('',#15794,10.);
#2455=VECTOR('',#15799,10.);
#2456=VECTOR('',#15800,10.);
#2457=VECTOR('',#15801,10.);
#2458=VECTOR('',#15806,10.);
#2459=VECTOR('',#15815,10.);
#2460=VECTOR('',#15818,10.);
#2461=VECTOR('',#15819,10.);
#2462=VECTOR('',#15820,10.);
#2463=VECTOR('',#15823,10.);
#2464=VECTOR('',#15824,10.);
#2465=VECTOR('',#15825,10.);
#2466=VECTOR('',#15826,10.);
#2467=VECTOR('',#15833,10.);
#2468=VECTOR('',#15836,10.);
#2469=VECTOR('',#15837,10.);
#2470=VECTOR('',#15838,10.);
#2471=VECTOR('',#15841,10.);
#2472=VECTOR('',#15842,10.);
#2473=VECTOR('',#15843,10.);
#2474=VECTOR('',#15844,10.);
#2475=VECTOR('',#15851,10.);
#2476=VECTOR('',#15854,10.);
#2477=VECTOR('',#15855,10.);
#2478=VECTOR('',#15856,10.);
#2479=VECTOR('',#15865,10.);
#2480=VECTOR('',#15866,10.);
#2481=VECTOR('',#15867,10.);
#2482=VECTOR('',#15876,10.);
#2483=VECTOR('',#15877,10.);
#2484=VECTOR('',#15878,10.);
#2485=VECTOR('',#15881,10.);
#2486=VECTOR('',#15882,10.);
#2487=VECTOR('',#15883,10.);
#2488=VECTOR('',#15886,10.);
#2489=VECTOR('',#15887,10.);
#2490=VECTOR('',#15892,10.);
#2491=VECTOR('',#15897,10.);
#2492=VECTOR('',#15898,10.);
#2493=VECTOR('',#15899,10.);
#2494=VECTOR('',#15904,10.);
#2495=VECTOR('',#15909,10.);
#2496=VECTOR('',#15910,10.);
#2497=VECTOR('',#15911,10.);
#2498=VECTOR('',#15914,10.);
#2499=VECTOR('',#15915,10.);
#2500=VECTOR('',#15916,10.);
#2501=VECTOR('',#15919,10.);
#2502=VECTOR('',#15920,10.);
#2503=VECTOR('',#15921,10.);
#2504=VECTOR('',#15926,10.);
#2505=VECTOR('',#15931,10.);
#2506=VECTOR('',#15932,10.);
#2507=VECTOR('',#15933,10.);
#2508=VECTOR('',#15938,10.);
#2509=VECTOR('',#15943,10.);
#2510=VECTOR('',#15944,10.);
#2511=VECTOR('',#15945,10.);
#2512=VECTOR('',#15952,10.);
#2513=VECTOR('',#15955,10.);
#2514=VECTOR('',#15956,10.);
#2515=VECTOR('',#15957,10.);
#2516=VECTOR('',#15964,10.);
#2517=VECTOR('',#15967,10.);
#2518=VECTOR('',#15968,10.);
#2519=VECTOR('',#15969,10.);
#2520=VECTOR('',#15972,10.);
#2521=VECTOR('',#15973,10.);
#2522=VECTOR('',#15974,10.);
#2523=VECTOR('',#15977,10.);
#2524=VECTOR('',#15978,10.);
#2525=VECTOR('',#15979,10.);
#2526=VECTOR('',#15986,10.);
#2527=VECTOR('',#15989,10.);
#2528=VECTOR('',#15990,10.);
#2529=VECTOR('',#15991,10.);
#2530=VECTOR('',#16008,1.49999999999999);
#2531=VECTOR('',#16013,10.);
#2532=VECTOR('',#16014,10.);
#2533=VECTOR('',#16015,10.);
#2534=VECTOR('',#16016,10.);
#2535=VECTOR('',#16019,10.);
#2536=VECTOR('',#16020,10.);
#2537=VECTOR('',#16021,10.);
#2538=VECTOR('',#16024,10.);
#2539=VECTOR('',#16025,10.);
#2540=VECTOR('',#16026,10.);
#2541=VECTOR('',#16029,10.);
#2542=VECTOR('',#16030,10.);
#2543=VECTOR('',#16031,10.);
#2544=VECTOR('',#16034,10.);
#2545=VECTOR('',#16035,10.);
#2546=VECTOR('',#16036,10.);
#2547=VECTOR('',#16039,10.);
#2548=VECTOR('',#16040,10.);
#2549=CYLINDRICAL_SURFACE('',#11490,21.2480593298244);
#2550=CYLINDRICAL_SURFACE('',#11502,21.2480593298244);
#2551=CYLINDRICAL_SURFACE('',#11509,6.);
#2552=CYLINDRICAL_SURFACE('',#11516,21.2480593298244);
#2553=CYLINDRICAL_SURFACE('',#11526,20.7480593298244);
#2554=CYLINDRICAL_SURFACE('',#11536,20.7480593298244);
#2555=CYLINDRICAL_SURFACE('',#11537,16.7480593298244);
#2556=CYLINDRICAL_SURFACE('',#11541,20.7480593298244);
#2557=CYLINDRICAL_SURFACE('',#11545,15.7480593298244);
#2558=CYLINDRICAL_SURFACE('',#11547,15.7480593298244);
#2559=CYLINDRICAL_SURFACE('',#11549,16.7480593298244);
#2560=CYLINDRICAL_SURFACE('',#11552,6.);
#2561=CYLINDRICAL_SURFACE('',#11556,1.);
#2562=CYLINDRICAL_SURFACE('',#11573,1.);
#2563=CYLINDRICAL_SURFACE('',#11575,2.5);
#2564=CYLINDRICAL_SURFACE('',#11578,2.5);
#2565=CYLINDRICAL_SURFACE('',#11581,2.5);
#2566=CYLINDRICAL_SURFACE('',#11584,7.5);
#2567=CYLINDRICAL_SURFACE('',#11587,2.5);
#2568=CYLINDRICAL_SURFACE('',#11590,2.5);
#2569=CYLINDRICAL_SURFACE('',#11593,2.5);
#2570=CYLINDRICAL_SURFACE('',#11596,2.5);
#2571=CYLINDRICAL_SURFACE('',#11599,2.5);
#2572=CYLINDRICAL_SURFACE('',#11602,2.5);
#2573=CYLINDRICAL_SURFACE('',#11605,2.5);
#2574=CYLINDRICAL_SURFACE('',#11608,2.5);
#2575=CYLINDRICAL_SURFACE('',#11610,2.5);
#2576=CYLINDRICAL_SURFACE('',#11612,2.5);
#2577=CYLINDRICAL_SURFACE('',#11614,2.5);
#2578=CYLINDRICAL_SURFACE('',#11616,2.5);
#2579=CYLINDRICAL_SURFACE('',#11618,2.5);
#2580=CYLINDRICAL_SURFACE('',#11620,2.5);
#2581=CYLINDRICAL_SURFACE('',#11622,7.5);
#2582=CYLINDRICAL_SURFACE('',#11624,2.5);
#2583=CYLINDRICAL_SURFACE('',#11626,2.5);
#2584=CYLINDRICAL_SURFACE('',#11628,2.5);
#2585=CYLINDRICAL_SURFACE('',#11630,2.5);
#2586=CYLINDRICAL_SURFACE('',#11633,2.5);
#2587=CYLINDRICAL_SURFACE('',#11636,2.5);
#2588=CYLINDRICAL_SURFACE('',#11639,7.5);
#2589=CYLINDRICAL_SURFACE('',#11642,2.5);
#2590=CYLINDRICAL_SURFACE('',#11645,2.5);
#2591=CYLINDRICAL_SURFACE('',#11648,2.5);
#2592=CYLINDRICAL_SURFACE('',#11651,2.5);
#2593=CYLINDRICAL_SURFACE('',#11654,2.5);
#2594=CYLINDRICAL_SURFACE('',#11657,2.5);
#2595=CYLINDRICAL_SURFACE('',#11660,2.5);
#2596=CYLINDRICAL_SURFACE('',#11681,1.4635);
#2597=CYLINDRICAL_SURFACE('',#11686,0.999999999999975);
#2598=CYLINDRICAL_SURFACE('',#11691,1.99999999999998);
#2599=CYLINDRICAL_SURFACE('',#11695,0.500000000000007);
#2600=CYLINDRICAL_SURFACE('',#11698,0.499999999999998);
#2601=CYLINDRICAL_SURFACE('',#11703,0.999999999999975);
#2602=CYLINDRICAL_SURFACE('',#11708,1.99999999999998);
#2603=CYLINDRICAL_SURFACE('',#11712,0.500000000000007);
#2604=CYLINDRICAL_SURFACE('',#11716,0.499999999999998);
#2605=CYLINDRICAL_SURFACE('',#11722,0.999999999999981);
#2606=CYLINDRICAL_SURFACE('',#11726,0.999999999999967);
#2607=CYLINDRICAL_SURFACE('',#11732,1.99999999999997);
#2608=CYLINDRICAL_SURFACE('',#11736,1.99999999999998);
#2609=CYLINDRICAL_SURFACE('',#11740,0.999999999999981);
#2610=CYLINDRICAL_SURFACE('',#11744,0.999999999999967);
#2611=CYLINDRICAL_SURFACE('',#11750,1.99999999999997);
#2612=CYLINDRICAL_SURFACE('',#11754,1.99999999999998);
#2613=CYLINDRICAL_SURFACE('',#11760,2.5);
#2614=CYLINDRICAL_SURFACE('',#11763,2.5);
#2615=CYLINDRICAL_SURFACE('',#11766,2.5);
#2616=CYLINDRICAL_SURFACE('',#11769,2.5);
#2617=CYLINDRICAL_SURFACE('',#11772,10.);
#2618=CYLINDRICAL_SURFACE('',#11776,1.5);
#2619=CYLINDRICAL_SURFACE('',#11780,1.5);
#2620=CYLINDRICAL_SURFACE('',#11784,1.5);
#2621=CYLINDRICAL_SURFACE('',#11788,1.5);
#2622=CYLINDRICAL_SURFACE('',#11791,2.5);
#2623=CYLINDRICAL_SURFACE('',#11794,2.5);
#2624=CYLINDRICAL_SURFACE('',#11797,2.5);
#2625=CYLINDRICAL_SURFACE('',#11800,2.5);
#2626=CYLINDRICAL_SURFACE('',#11803,10.);
#2627=CYLINDRICAL_SURFACE('',#11807,1.5);
#2628=CYLINDRICAL_SURFACE('',#11811,1.5);
#2629=CYLINDRICAL_SURFACE('',#11815,1.5);
#2630=CYLINDRICAL_SURFACE('',#11819,1.5);
#2631=CYLINDRICAL_SURFACE('',#11822,2.5);
#2632=CYLINDRICAL_SURFACE('',#11825,2.5);
#2633=CYLINDRICAL_SURFACE('',#11828,2.5);
#2634=CYLINDRICAL_SURFACE('',#11831,2.5);
#2635=CYLINDRICAL_SURFACE('',#11834,10.);
#2636=CYLINDRICAL_SURFACE('',#11838,1.5);
#2637=CYLINDRICAL_SURFACE('',#11842,1.5);
#2638=CYLINDRICAL_SURFACE('',#11846,1.5);
#2639=CYLINDRICAL_SURFACE('',#11850,1.5);
#2640=CYLINDRICAL_SURFACE('',#11853,2.5);
#2641=CYLINDRICAL_SURFACE('',#11856,2.5);
#2642=CYLINDRICAL_SURFACE('',#11859,2.5);
#2643=CYLINDRICAL_SURFACE('',#11862,2.5);
#2644=CYLINDRICAL_SURFACE('',#11865,10.);
#2645=CYLINDRICAL_SURFACE('',#11869,1.5);
#2646=CYLINDRICAL_SURFACE('',#11873,1.5);
#2647=CYLINDRICAL_SURFACE('',#11877,1.5);
#2648=CYLINDRICAL_SURFACE('',#11881,1.5);
#2649=CYLINDRICAL_SURFACE('',#11884,2.5);
#2650=CYLINDRICAL_SURFACE('',#11887,2.5);
#2651=CYLINDRICAL_SURFACE('',#11890,2.5);
#2652=CYLINDRICAL_SURFACE('',#11893,2.5);
#2653=CYLINDRICAL_SURFACE('',#11896,10.);
#2654=CYLINDRICAL_SURFACE('',#11900,1.5);
#2655=CYLINDRICAL_SURFACE('',#11904,1.5);
#2656=CYLINDRICAL_SURFACE('',#11908,1.5);
#2657=CYLINDRICAL_SURFACE('',#11912,1.5);
#2658=CYLINDRICAL_SURFACE('',#11915,2.5);
#2659=CYLINDRICAL_SURFACE('',#11918,2.5);
#2660=CYLINDRICAL_SURFACE('',#11921,2.5);
#2661=CYLINDRICAL_SURFACE('',#11924,2.5);
#2662=CYLINDRICAL_SURFACE('',#11927,10.);
#2663=CYLINDRICAL_SURFACE('',#11931,1.5);
#2664=CYLINDRICAL_SURFACE('',#11935,1.5);
#2665=CYLINDRICAL_SURFACE('',#11939,1.5);
#2666=CYLINDRICAL_SURFACE('',#11943,1.5);
#2667=CYLINDRICAL_SURFACE('',#11946,2.5);
#2668=CYLINDRICAL_SURFACE('',#11949,2.5);
#2669=CYLINDRICAL_SURFACE('',#11952,2.5);
#2670=CYLINDRICAL_SURFACE('',#11955,2.5);
#2671=CYLINDRICAL_SURFACE('',#11958,10.);
#2672=CYLINDRICAL_SURFACE('',#11962,1.5);
#2673=CYLINDRICAL_SURFACE('',#11966,1.5);
#2674=CYLINDRICAL_SURFACE('',#11970,1.5);
#2675=CYLINDRICAL_SURFACE('',#11974,1.5);
#2676=CYLINDRICAL_SURFACE('',#11977,2.5);
#2677=CYLINDRICAL_SURFACE('',#11980,2.5);
#2678=CYLINDRICAL_SURFACE('',#11983,2.5);
#2679=CYLINDRICAL_SURFACE('',#11986,2.5);
#2680=CYLINDRICAL_SURFACE('',#11989,10.);
#2681=CYLINDRICAL_SURFACE('',#11993,1.5);
#2682=CYLINDRICAL_SURFACE('',#11997,1.5);
#2683=CYLINDRICAL_SURFACE('',#12001,1.5);
#2684=CYLINDRICAL_SURFACE('',#12005,1.5);
#2685=CYLINDRICAL_SURFACE('',#12008,2.5);
#2686=CYLINDRICAL_SURFACE('',#12011,2.5);
#2687=CYLINDRICAL_SURFACE('',#12014,2.5);
#2688=CYLINDRICAL_SURFACE('',#12017,2.5);
#2689=CYLINDRICAL_SURFACE('',#12020,10.);
#2690=CYLINDRICAL_SURFACE('',#12024,1.5);
#2691=CYLINDRICAL_SURFACE('',#12028,1.5);
#2692=CYLINDRICAL_SURFACE('',#12032,1.5);
#2693=CYLINDRICAL_SURFACE('',#12036,1.5);
#2694=CYLINDRICAL_SURFACE('',#12039,2.5);
#2695=CYLINDRICAL_SURFACE('',#12042,2.5);
#2696=CYLINDRICAL_SURFACE('',#12046,1.5);
#2697=CYLINDRICAL_SURFACE('',#12050,1.5);
#2698=CYLINDRICAL_SURFACE('',#12054,1.5);
#2699=CYLINDRICAL_SURFACE('',#12058,1.5);
#2700=CYLINDRICAL_SURFACE('',#12061,10.);
#2701=CYLINDRICAL_SURFACE('',#12064,2.5);
#2702=CYLINDRICAL_SURFACE('',#12067,2.5);
#2703=CYLINDRICAL_SURFACE('',#12070,0.5);
#2704=CYLINDRICAL_SURFACE('',#12074,0.5);
#2705=CYLINDRICAL_SURFACE('',#12125,2.);
#2706=CYLINDRICAL_SURFACE('',#12131,2.);
#2707=CYLINDRICAL_SURFACE('',#12133,2.);
#2708=CYLINDRICAL_SURFACE('',#12135,1.99999999999999);
#2709=CYLINDRICAL_SURFACE('',#12137,2.00000000000003);
#2710=CYLINDRICAL_SURFACE('',#12139,1.99999999999999);
#2711=CYLINDRICAL_SURFACE('',#12141,2.00000000000003);
#2712=CYLINDRICAL_SURFACE('',#12143,2.);
#2713=CYLINDRICAL_SURFACE('',#12145,1.99999999999999);
#2714=CYLINDRICAL_SURFACE('',#12147,1.99999999999999);
#2715=CYLINDRICAL_SURFACE('',#12149,1.99999999999999);
#2716=CYLINDRICAL_SURFACE('',#12151,1.99999999999999);
#2717=CYLINDRICAL_SURFACE('',#12153,1.99999999999999);
#2718=CYLINDRICAL_SURFACE('',#12155,1.99999999999999);
#2719=CYLINDRICAL_SURFACE('',#12157,2.);
#2720=CYLINDRICAL_SURFACE('',#12159,1.99999999999999);
#2721=CYLINDRICAL_SURFACE('',#12161,1.99999999999999);
#2722=CYLINDRICAL_SURFACE('',#12163,1.99999999999999);
#2723=CYLINDRICAL_SURFACE('',#12165,1.99999999999999);
#2724=CYLINDRICAL_SURFACE('',#12167,2.);
#2725=CYLINDRICAL_SURFACE('',#12169,2.);
#2726=CYLINDRICAL_SURFACE('',#12171,2.00000000000003);
#2727=CYLINDRICAL_SURFACE('',#12173,2.);
#2728=CYLINDRICAL_SURFACE('',#12175,1.99999999999999);
#2729=CYLINDRICAL_SURFACE('',#12177,2.);
#2730=CYLINDRICAL_SURFACE('',#12179,1.99999999999999);
#2731=CYLINDRICAL_SURFACE('',#12181,1.99999999999999);
#2732=CYLINDRICAL_SURFACE('',#12183,1.99999999999999);
#2733=CYLINDRICAL_SURFACE('',#12185,1.99999999999999);
#2734=CYLINDRICAL_SURFACE('',#12187,1.99999999999999);
#2735=CYLINDRICAL_SURFACE('',#12189,1.99999999999999);
#2736=CYLINDRICAL_SURFACE('',#12191,1.99999999999999);
#2737=CYLINDRICAL_SURFACE('',#12193,2.);
#2738=CYLINDRICAL_SURFACE('',#12195,2.00000000000003);
#2739=CYLINDRICAL_SURFACE('',#12197,1.99999999999999);
#2740=CYLINDRICAL_SURFACE('',#12199,1.99999999999999);
#2741=CYLINDRICAL_SURFACE('',#12201,1.99999999999999);
#2742=CYLINDRICAL_SURFACE('',#12203,1.99999999999999);
#2743=CYLINDRICAL_SURFACE('',#12205,2.);
#2744=CYLINDRICAL_SURFACE('',#12207,2.00000000000003);
#2745=CYLINDRICAL_SURFACE('',#12209,2.00000000000003);
#2746=CYLINDRICAL_SURFACE('',#12211,2.00000000000003);
#2747=CYLINDRICAL_SURFACE('',#12213,1.99999999999999);
#2748=CYLINDRICAL_SURFACE('',#12215,1.99999999999999);
#2749=CYLINDRICAL_SURFACE('',#12217,1.99999999999999);
#2750=CYLINDRICAL_SURFACE('',#12219,2.00000000000003);
#2751=CYLINDRICAL_SURFACE('',#12221,1.99999999999999);
#2752=CYLINDRICAL_SURFACE('',#12223,1.99999999999999);
#2753=CYLINDRICAL_SURFACE('',#12225,1.99999999999999);
#2754=CYLINDRICAL_SURFACE('',#12229,2.);
#2755=CYLINDRICAL_SURFACE('',#12232,1.99999999999999);
#2756=CYLINDRICAL_SURFACE('',#12235,2.00000000000003);
#2757=CYLINDRICAL_SURFACE('',#12238,1.99999999999999);
#2758=CYLINDRICAL_SURFACE('',#12241,2.00000000000003);
#2759=CYLINDRICAL_SURFACE('',#12244,2.);
#2760=CYLINDRICAL_SURFACE('',#12247,1.99999999999999);
#2761=CYLINDRICAL_SURFACE('',#12250,1.99999999999999);
#2762=CYLINDRICAL_SURFACE('',#12253,1.99999999999999);
#2763=CYLINDRICAL_SURFACE('',#12256,1.99999999999999);
#2764=CYLINDRICAL_SURFACE('',#12259,1.99999999999999);
#2765=CYLINDRICAL_SURFACE('',#12262,1.99999999999999);
#2766=CYLINDRICAL_SURFACE('',#12265,2.);
#2767=CYLINDRICAL_SURFACE('',#12268,1.99999999999999);
#2768=CYLINDRICAL_SURFACE('',#12271,1.99999999999999);
#2769=CYLINDRICAL_SURFACE('',#12274,1.99999999999999);
#2770=CYLINDRICAL_SURFACE('',#12277,1.99999999999999);
#2771=CYLINDRICAL_SURFACE('',#12280,2.);
#2772=CYLINDRICAL_SURFACE('',#12283,2.);
#2773=CYLINDRICAL_SURFACE('',#12286,2.00000000000003);
#2774=CYLINDRICAL_SURFACE('',#12289,2.);
#2775=CYLINDRICAL_SURFACE('',#12292,1.99999999999999);
#2776=CYLINDRICAL_SURFACE('',#12295,2.);
#2777=CYLINDRICAL_SURFACE('',#12298,1.99999999999999);
#2778=CYLINDRICAL_SURFACE('',#12301,1.99999999999999);
#2779=CYLINDRICAL_SURFACE('',#12304,1.99999999999999);
#2780=CYLINDRICAL_SURFACE('',#12307,1.99999999999999);
#2781=CYLINDRICAL_SURFACE('',#12310,1.99999999999999);
#2782=CYLINDRICAL_SURFACE('',#12313,1.99999999999999);
#2783=CYLINDRICAL_SURFACE('',#12316,1.99999999999999);
#2784=CYLINDRICAL_SURFACE('',#12319,2.);
#2785=CYLINDRICAL_SURFACE('',#12322,2.00000000000003);
#2786=CYLINDRICAL_SURFACE('',#12325,1.99999999999999);
#2787=CYLINDRICAL_SURFACE('',#12328,1.99999999999999);
#2788=CYLINDRICAL_SURFACE('',#12331,1.99999999999999);
#2789=CYLINDRICAL_SURFACE('',#12334,1.99999999999999);
#2790=CYLINDRICAL_SURFACE('',#12337,2.);
#2791=CYLINDRICAL_SURFACE('',#12340,2.00000000000003);
#2792=CYLINDRICAL_SURFACE('',#12343,2.00000000000003);
#2793=CYLINDRICAL_SURFACE('',#12346,2.00000000000003);
#2794=CYLINDRICAL_SURFACE('',#12349,1.99999999999999);
#2795=CYLINDRICAL_SURFACE('',#12352,1.99999999999999);
#2796=CYLINDRICAL_SURFACE('',#12355,1.99999999999999);
#2797=CYLINDRICAL_SURFACE('',#12358,2.00000000000003);
#2798=CYLINDRICAL_SURFACE('',#12361,1.99999999999999);
#2799=CYLINDRICAL_SURFACE('',#12364,1.99999999999999);
#2800=CYLINDRICAL_SURFACE('',#12367,1.99999999999999);
#2801=CYLINDRICAL_SURFACE('',#12375,1.49999999999999);
#2802=CYLINDRICAL_SURFACE('',#12378,2.00000000000003);
#2803=CYLINDRICAL_SURFACE('',#12381,2.00000000000003);
#2804=CYLINDRICAL_SURFACE('',#12384,2.);
#2805=CYLINDRICAL_SURFACE('',#12399,4.);
#2806=CYLINDRICAL_SURFACE('',#12414,1.49999999999999);
#2807=CYLINDRICAL_SURFACE('',#12415,1.49999999999999);
#2808=CYLINDRICAL_SURFACE('',#12416,1.49999999999999);
#2809=CYLINDRICAL_SURFACE('',#12417,1.49999999999999);
#2810=CYLINDRICAL_SURFACE('',#12418,1.49999999999999);
#2811=CYLINDRICAL_SURFACE('',#12419,1.49999999999999);
#2812=CYLINDRICAL_SURFACE('',#12420,1.49999999999999);
#2813=CYLINDRICAL_SURFACE('',#12421,1.49999999999999);
#2814=CYLINDRICAL_SURFACE('',#12422,1.49999999999999);
#2815=CYLINDRICAL_SURFACE('',#12423,1.49999999999999);
#2816=CYLINDRICAL_SURFACE('',#12424,1.49999999999999);
#2817=CYLINDRICAL_SURFACE('',#12442,1.49999999999999);
#2818=CYLINDRICAL_SURFACE('',#12444,1.49999999999999);
#2819=CYLINDRICAL_SURFACE('',#12446,1.49999999999999);
#2820=CYLINDRICAL_SURFACE('',#12448,1.49999999999999);
#2821=CYLINDRICAL_SURFACE('',#12450,1.49999999999999);
#2822=CYLINDRICAL_SURFACE('',#12452,1.49999999999999);
#2823=CYLINDRICAL_SURFACE('',#12454,1.49999999999999);
#2824=CYLINDRICAL_SURFACE('',#12456,1.49999999999999);
#2825=CYLINDRICAL_SURFACE('',#12458,1.49999999999999);
#2826=CYLINDRICAL_SURFACE('',#12460,1.49999999999999);
#2827=CYLINDRICAL_SURFACE('',#12462,1.49999999999999);
#2828=CYLINDRICAL_SURFACE('',#12477,1.465);
#2829=CYLINDRICAL_SURFACE('',#12489,1.5);
#2830=CYLINDRICAL_SURFACE('',#12492,2.00000000000003);
#2831=CYLINDRICAL_SURFACE('',#12495,2.00000000000003);
#2832=CYLINDRICAL_SURFACE('',#12498,2.);
#2833=CYLINDRICAL_SURFACE('',#12513,4.);
#2834=CYLINDRICAL_SURFACE('',#12528,1.49999999999999);
#2835=CYLINDRICAL_SURFACE('',#12529,1.49999999999999);
#2836=CYLINDRICAL_SURFACE('',#12530,1.49999999999999);
#2837=CYLINDRICAL_SURFACE('',#12531,1.49999999999999);
#2838=CYLINDRICAL_SURFACE('',#12532,1.49999999999999);
#2839=CYLINDRICAL_SURFACE('',#12533,1.49999999999999);
#2840=CYLINDRICAL_SURFACE('',#12534,1.49999999999999);
#2841=CYLINDRICAL_SURFACE('',#12535,1.49999999999999);
#2842=CYLINDRICAL_SURFACE('',#12536,1.49999999999999);
#2843=CYLINDRICAL_SURFACE('',#12537,1.49999999999999);
#2844=CYLINDRICAL_SURFACE('',#12538,1.49999999999999);
#2845=CYLINDRICAL_SURFACE('',#12556,1.49999999999999);
#2846=CYLINDRICAL_SURFACE('',#12558,1.49999999999999);
#2847=CYLINDRICAL_SURFACE('',#12560,1.49999999999999);
#2848=CYLINDRICAL_SURFACE('',#12562,1.49999999999999);
#2849=CYLINDRICAL_SURFACE('',#12564,1.49999999999999);
#2850=CYLINDRICAL_SURFACE('',#12566,1.49999999999999);
#2851=CYLINDRICAL_SURFACE('',#12568,1.49999999999999);
#2852=CYLINDRICAL_SURFACE('',#12570,1.49999999999999);
#2853=CYLINDRICAL_SURFACE('',#12572,1.49999999999999);
#2854=CYLINDRICAL_SURFACE('',#12574,1.49999999999999);
#2855=CYLINDRICAL_SURFACE('',#12576,1.49999999999999);
#2856=CYLINDRICAL_SURFACE('',#12600,1.4635);
#2857=CYLINDRICAL_SURFACE('',#12604,1.465);
#2858=CYLINDRICAL_SURFACE('',#12616,1.465);
#2859=CYLINDRICAL_SURFACE('',#12629,0.999999999999975);
#2860=CYLINDRICAL_SURFACE('',#12634,1.99999999999998);
#2861=CYLINDRICAL_SURFACE('',#12638,0.500000000000007);
#2862=CYLINDRICAL_SURFACE('',#12641,0.499999999999998);
#2863=CYLINDRICAL_SURFACE('',#12646,0.999999999999975);
#2864=CYLINDRICAL_SURFACE('',#12651,1.99999999999998);
#2865=CYLINDRICAL_SURFACE('',#12655,0.500000000000007);
#2866=CYLINDRICAL_SURFACE('',#12659,0.499999999999998);
#2867=CYLINDRICAL_SURFACE('',#12665,0.999999999999981);
#2868=CYLINDRICAL_SURFACE('',#12669,0.999999999999967);
#2869=CYLINDRICAL_SURFACE('',#12675,1.99999999999997);
#2870=CYLINDRICAL_SURFACE('',#12679,1.99999999999998);
#2871=CYLINDRICAL_SURFACE('',#12683,0.999999999999981);
#2872=CYLINDRICAL_SURFACE('',#12687,0.999999999999967);
#2873=CYLINDRICAL_SURFACE('',#12693,1.99999999999997);
#2874=CYLINDRICAL_SURFACE('',#12697,1.99999999999998);
#2875=CYLINDRICAL_SURFACE('',#12703,1.465);
#2876=STYLED_ITEM('',(#19417),#10769);
#2877=STYLED_ITEM('',(#19417),#10773);
#2878=STYLED_ITEM('',(#19417),#95);
#2879=STYLED_ITEM('',(#19389),#96);
#2880=STYLED_ITEM('',(#19417),#97);
#2881=STYLED_ITEM('',(#19410),#98);
#2882=STYLED_ITEM('',(#19396),#99);
#2883=STYLED_ITEM('',(#19382),#100);
#2884=STYLED_ITEM('',(#19382),#101);
#2885=STYLED_ITEM('',(#19410),#102);
#2886=STYLED_ITEM('',(#19382),#103);
#2887=STYLED_ITEM('',(#19410),#104);
#2888=STYLED_ITEM('',(#19410),#105);
#2889=STYLED_ITEM('',(#19410),#106);
#2890=STYLED_ITEM('',(#19389),#107);
#2891=STYLED_ITEM('',(#19410),#108);
#2892=FACE_OUTER_BOUND('',#3438,.T.);
#2893=FACE_OUTER_BOUND('',#3439,.T.);
#2894=FACE_OUTER_BOUND('',#3440,.T.);
#2895=FACE_OUTER_BOUND('',#3441,.T.);
#2896=FACE_OUTER_BOUND('',#3442,.T.);
#2897=FACE_OUTER_BOUND('',#3443,.T.);
#2898=FACE_OUTER_BOUND('',#3444,.T.);
#2899=FACE_OUTER_BOUND('',#3445,.T.);
#2900=FACE_OUTER_BOUND('',#3446,.T.);
#2901=FACE_OUTER_BOUND('',#3447,.T.);
#2902=FACE_OUTER_BOUND('',#3448,.T.);
#2903=FACE_OUTER_BOUND('',#3449,.T.);
#2904=FACE_OUTER_BOUND('',#3451,.T.);
#2905=FACE_OUTER_BOUND('',#3452,.T.);
#2906=FACE_OUTER_BOUND('',#3454,.T.);
#2907=FACE_OUTER_BOUND('',#3455,.T.);
#2908=FACE_OUTER_BOUND('',#3457,.T.);
#2909=FACE_OUTER_BOUND('',#3459,.T.);
#2910=FACE_OUTER_BOUND('',#3461,.T.);
#2911=FACE_OUTER_BOUND('',#3462,.T.);
#2912=FACE_OUTER_BOUND('',#3463,.T.);
#2913=FACE_OUTER_BOUND('',#3465,.T.);
#2914=FACE_OUTER_BOUND('',#3466,.T.);
#2915=FACE_OUTER_BOUND('',#3468,.T.);
#2916=FACE_OUTER_BOUND('',#3469,.T.);
#2917=FACE_OUTER_BOUND('',#3470,.T.);
#2918=FACE_OUTER_BOUND('',#3471,.T.);
#2919=FACE_OUTER_BOUND('',#3473,.T.);
#2920=FACE_OUTER_BOUND('',#3474,.T.);
#2921=FACE_OUTER_BOUND('',#3476,.T.);
#2922=FACE_OUTER_BOUND('',#3477,.T.);
#2923=FACE_OUTER_BOUND('',#3489,.T.);
#2924=FACE_OUTER_BOUND('',#3490,.T.);
#2925=FACE_OUTER_BOUND('',#3491,.T.);
#2926=FACE_OUTER_BOUND('',#3492,.T.);
#2927=FACE_OUTER_BOUND('',#3493,.T.);
#2928=FACE_OUTER_BOUND('',#3494,.T.);
#2929=FACE_OUTER_BOUND('',#3495,.T.);
#2930=FACE_OUTER_BOUND('',#3496,.T.);
#2931=FACE_OUTER_BOUND('',#3497,.T.);
#2932=FACE_OUTER_BOUND('',#3498,.T.);
#2933=FACE_OUTER_BOUND('',#3499,.T.);
#2934=FACE_OUTER_BOUND('',#3500,.T.);
#2935=FACE_OUTER_BOUND('',#3501,.T.);
#2936=FACE_OUTER_BOUND('',#3502,.T.);
#2937=FACE_OUTER_BOUND('',#3503,.T.);
#2938=FACE_OUTER_BOUND('',#3504,.T.);
#2939=FACE_OUTER_BOUND('',#3505,.T.);
#2940=FACE_OUTER_BOUND('',#3506,.T.);
#2941=FACE_OUTER_BOUND('',#3507,.T.);
#2942=FACE_OUTER_BOUND('',#3508,.T.);
#2943=FACE_OUTER_BOUND('',#3509,.T.);
#2944=FACE_OUTER_BOUND('',#3510,.T.);
#2945=FACE_OUTER_BOUND('',#3511,.T.);
#2946=FACE_OUTER_BOUND('',#3512,.T.);
#2947=FACE_OUTER_BOUND('',#3513,.T.);
#2948=FACE_OUTER_BOUND('',#3514,.T.);
#2949=FACE_OUTER_BOUND('',#3515,.T.);
#2950=FACE_OUTER_BOUND('',#3516,.T.);
#2951=FACE_OUTER_BOUND('',#3517,.T.);
#2952=FACE_OUTER_BOUND('',#3518,.T.);
#2953=FACE_OUTER_BOUND('',#3519,.T.);
#2954=FACE_OUTER_BOUND('',#3520,.T.);
#2955=FACE_OUTER_BOUND('',#3521,.T.);
#2956=FACE_OUTER_BOUND('',#3522,.T.);
#2957=FACE_OUTER_BOUND('',#3523,.T.);
#2958=FACE_OUTER_BOUND('',#3524,.T.);
#2959=FACE_OUTER_BOUND('',#3525,.T.);
#2960=FACE_OUTER_BOUND('',#3537,.T.);
#2961=FACE_OUTER_BOUND('',#3549,.T.);
#2962=FACE_OUTER_BOUND('',#3550,.T.);
#2963=FACE_OUTER_BOUND('',#3562,.T.);
#2964=FACE_OUTER_BOUND('',#3574,.T.);
#2965=FACE_OUTER_BOUND('',#3586,.T.);
#2966=FACE_OUTER_BOUND('',#3587,.T.);
#2967=FACE_OUTER_BOUND('',#3589,.T.);
#2968=FACE_OUTER_BOUND('',#3590,.T.);
#2969=FACE_OUTER_BOUND('',#3591,.T.);
#2970=FACE_OUTER_BOUND('',#3592,.T.);
#2971=FACE_OUTER_BOUND('',#3593,.T.);
#2972=FACE_OUTER_BOUND('',#3594,.T.);
#2973=FACE_OUTER_BOUND('',#3595,.T.);
#2974=FACE_OUTER_BOUND('',#3596,.T.);
#2975=FACE_OUTER_BOUND('',#3597,.T.);
#2976=FACE_OUTER_BOUND('',#3598,.T.);
#2977=FACE_OUTER_BOUND('',#3599,.T.);
#2978=FACE_OUTER_BOUND('',#3600,.T.);
#2979=FACE_OUTER_BOUND('',#3601,.T.);
#2980=FACE_OUTER_BOUND('',#3602,.T.);
#2981=FACE_OUTER_BOUND('',#3603,.T.);
#2982=FACE_OUTER_BOUND('',#3604,.T.);
#2983=FACE_OUTER_BOUND('',#3605,.T.);
#2984=FACE_OUTER_BOUND('',#3606,.T.);
#2985=FACE_OUTER_BOUND('',#3607,.T.);
#2986=FACE_OUTER_BOUND('',#3608,.T.);
#2987=FACE_OUTER_BOUND('',#3609,.T.);
#2988=FACE_OUTER_BOUND('',#3610,.T.);
#2989=FACE_OUTER_BOUND('',#3611,.T.);
#2990=FACE_OUTER_BOUND('',#3612,.T.);
#2991=FACE_OUTER_BOUND('',#3613,.T.);
#2992=FACE_OUTER_BOUND('',#3614,.T.);
#2993=FACE_OUTER_BOUND('',#3615,.T.);
#2994=FACE_OUTER_BOUND('',#3616,.T.);
#2995=FACE_OUTER_BOUND('',#3617,.T.);
#2996=FACE_OUTER_BOUND('',#3618,.T.);
#2997=FACE_OUTER_BOUND('',#3619,.T.);
#2998=FACE_OUTER_BOUND('',#3620,.T.);
#2999=FACE_OUTER_BOUND('',#3621,.T.);
#3000=FACE_OUTER_BOUND('',#3622,.T.);
#3001=FACE_OUTER_BOUND('',#3623,.T.);
#3002=FACE_OUTER_BOUND('',#3624,.T.);
#3003=FACE_OUTER_BOUND('',#3625,.T.);
#3004=FACE_OUTER_BOUND('',#3626,.T.);
#3005=FACE_OUTER_BOUND('',#3627,.T.);
#3006=FACE_OUTER_BOUND('',#3628,.T.);
#3007=FACE_OUTER_BOUND('',#3629,.T.);
#3008=FACE_OUTER_BOUND('',#3630,.T.);
#3009=FACE_OUTER_BOUND('',#3631,.T.);
#3010=FACE_OUTER_BOUND('',#3632,.T.);
#3011=FACE_OUTER_BOUND('',#3633,.T.);
#3012=FACE_OUTER_BOUND('',#3634,.T.);
#3013=FACE_OUTER_BOUND('',#3635,.T.);
#3014=FACE_OUTER_BOUND('',#3636,.T.);
#3015=FACE_OUTER_BOUND('',#3637,.T.);
#3016=FACE_OUTER_BOUND('',#3638,.T.);
#3017=FACE_OUTER_BOUND('',#3640,.T.);
#3018=FACE_OUTER_BOUND('',#3642,.T.);
#3019=FACE_OUTER_BOUND('',#3643,.T.);
#3020=FACE_OUTER_BOUND('',#3644,.T.);
#3021=FACE_OUTER_BOUND('',#3645,.T.);
#3022=FACE_OUTER_BOUND('',#3646,.T.);
#3023=FACE_OUTER_BOUND('',#3647,.T.);
#3024=FACE_OUTER_BOUND('',#3648,.T.);
#3025=FACE_OUTER_BOUND('',#3649,.T.);
#3026=FACE_OUTER_BOUND('',#3650,.T.);
#3027=FACE_OUTER_BOUND('',#3651,.T.);
#3028=FACE_OUTER_BOUND('',#3652,.T.);
#3029=FACE_OUTER_BOUND('',#3653,.T.);
#3030=FACE_OUTER_BOUND('',#3654,.T.);
#3031=FACE_OUTER_BOUND('',#3655,.T.);
#3032=FACE_OUTER_BOUND('',#3656,.T.);
#3033=FACE_OUTER_BOUND('',#3657,.T.);
#3034=FACE_OUTER_BOUND('',#3658,.T.);
#3035=FACE_OUTER_BOUND('',#3659,.T.);
#3036=FACE_OUTER_BOUND('',#3660,.T.);
#3037=FACE_OUTER_BOUND('',#3661,.T.);
#3038=FACE_OUTER_BOUND('',#3662,.T.);
#3039=FACE_OUTER_BOUND('',#3663,.T.);
#3040=FACE_OUTER_BOUND('',#3664,.T.);
#3041=FACE_OUTER_BOUND('',#3665,.T.);
#3042=FACE_OUTER_BOUND('',#3666,.T.);
#3043=FACE_OUTER_BOUND('',#3667,.T.);
#3044=FACE_OUTER_BOUND('',#3668,.T.);
#3045=FACE_OUTER_BOUND('',#3669,.T.);
#3046=FACE_OUTER_BOUND('',#3670,.T.);
#3047=FACE_OUTER_BOUND('',#3671,.T.);
#3048=FACE_OUTER_BOUND('',#3672,.T.);
#3049=FACE_OUTER_BOUND('',#3673,.T.);
#3050=FACE_OUTER_BOUND('',#3674,.T.);
#3051=FACE_OUTER_BOUND('',#3675,.T.);
#3052=FACE_OUTER_BOUND('',#3676,.T.);
#3053=FACE_OUTER_BOUND('',#3677,.T.);
#3054=FACE_OUTER_BOUND('',#3678,.T.);
#3055=FACE_OUTER_BOUND('',#3679,.T.);
#3056=FACE_OUTER_BOUND('',#3680,.T.);
#3057=FACE_OUTER_BOUND('',#3681,.T.);
#3058=FACE_OUTER_BOUND('',#3682,.T.);
#3059=FACE_OUTER_BOUND('',#3683,.T.);
#3060=FACE_OUTER_BOUND('',#3684,.T.);
#3061=FACE_OUTER_BOUND('',#3685,.T.);
#3062=FACE_OUTER_BOUND('',#3686,.T.);
#3063=FACE_OUTER_BOUND('',#3687,.T.);
#3064=FACE_OUTER_BOUND('',#3688,.T.);
#3065=FACE_OUTER_BOUND('',#3689,.T.);
#3066=FACE_OUTER_BOUND('',#3690,.T.);
#3067=FACE_OUTER_BOUND('',#3691,.T.);
#3068=FACE_OUTER_BOUND('',#3692,.T.);
#3069=FACE_OUTER_BOUND('',#3693,.T.);
#3070=FACE_OUTER_BOUND('',#3694,.T.);
#3071=FACE_OUTER_BOUND('',#3695,.T.);
#3072=FACE_OUTER_BOUND('',#3696,.T.);
#3073=FACE_OUTER_BOUND('',#3697,.T.);
#3074=FACE_OUTER_BOUND('',#3698,.T.);
#3075=FACE_OUTER_BOUND('',#3699,.T.);
#3076=FACE_OUTER_BOUND('',#3700,.T.);
#3077=FACE_OUTER_BOUND('',#3701,.T.);
#3078=FACE_OUTER_BOUND('',#3702,.T.);
#3079=FACE_OUTER_BOUND('',#3703,.T.);
#3080=FACE_OUTER_BOUND('',#3704,.T.);
#3081=FACE_OUTER_BOUND('',#3705,.T.);
#3082=FACE_OUTER_BOUND('',#3706,.T.);
#3083=FACE_OUTER_BOUND('',#3707,.T.);
#3084=FACE_OUTER_BOUND('',#3708,.T.);
#3085=FACE_OUTER_BOUND('',#3709,.T.);
#3086=FACE_OUTER_BOUND('',#3710,.T.);
#3087=FACE_OUTER_BOUND('',#3711,.T.);
#3088=FACE_OUTER_BOUND('',#3712,.T.);
#3089=FACE_OUTER_BOUND('',#3713,.T.);
#3090=FACE_OUTER_BOUND('',#3714,.T.);
#3091=FACE_OUTER_BOUND('',#3715,.T.);
#3092=FACE_OUTER_BOUND('',#3716,.T.);
#3093=FACE_OUTER_BOUND('',#3717,.T.);
#3094=FACE_OUTER_BOUND('',#3718,.T.);
#3095=FACE_OUTER_BOUND('',#3719,.T.);
#3096=FACE_OUTER_BOUND('',#3720,.T.);
#3097=FACE_OUTER_BOUND('',#3721,.T.);
#3098=FACE_OUTER_BOUND('',#3722,.T.);
#3099=FACE_OUTER_BOUND('',#3723,.T.);
#3100=FACE_OUTER_BOUND('',#3724,.T.);
#3101=FACE_OUTER_BOUND('',#3725,.T.);
#3102=FACE_OUTER_BOUND('',#3726,.T.);
#3103=FACE_OUTER_BOUND('',#3727,.T.);
#3104=FACE_OUTER_BOUND('',#3728,.T.);
#3105=FACE_OUTER_BOUND('',#3729,.T.);
#3106=FACE_OUTER_BOUND('',#3730,.T.);
#3107=FACE_OUTER_BOUND('',#3731,.T.);
#3108=FACE_OUTER_BOUND('',#3732,.T.);
#3109=FACE_OUTER_BOUND('',#3733,.T.);
#3110=FACE_OUTER_BOUND('',#3734,.T.);
#3111=FACE_OUTER_BOUND('',#3735,.T.);
#3112=FACE_OUTER_BOUND('',#3736,.T.);
#3113=FACE_OUTER_BOUND('',#3737,.T.);
#3114=FACE_OUTER_BOUND('',#3738,.T.);
#3115=FACE_OUTER_BOUND('',#3739,.T.);
#3116=FACE_OUTER_BOUND('',#3740,.T.);
#3117=FACE_OUTER_BOUND('',#3741,.T.);
#3118=FACE_OUTER_BOUND('',#3742,.T.);
#3119=FACE_OUTER_BOUND('',#3743,.T.);
#3120=FACE_OUTER_BOUND('',#3744,.T.);
#3121=FACE_OUTER_BOUND('',#3745,.T.);
#3122=FACE_OUTER_BOUND('',#3746,.T.);
#3123=FACE_OUTER_BOUND('',#3747,.T.);
#3124=FACE_OUTER_BOUND('',#3748,.T.);
#3125=FACE_OUTER_BOUND('',#3749,.T.);
#3126=FACE_OUTER_BOUND('',#3750,.T.);
#3127=FACE_OUTER_BOUND('',#3751,.T.);
#3128=FACE_OUTER_BOUND('',#3752,.T.);
#3129=FACE_OUTER_BOUND('',#3753,.T.);
#3130=FACE_OUTER_BOUND('',#3754,.T.);
#3131=FACE_OUTER_BOUND('',#3755,.T.);
#3132=FACE_OUTER_BOUND('',#3756,.T.);
#3133=FACE_OUTER_BOUND('',#3757,.T.);
#3134=FACE_OUTER_BOUND('',#3758,.T.);
#3135=FACE_OUTER_BOUND('',#3759,.T.);
#3136=FACE_OUTER_BOUND('',#3760,.T.);
#3137=FACE_OUTER_BOUND('',#3761,.T.);
#3138=FACE_OUTER_BOUND('',#3762,.T.);
#3139=FACE_OUTER_BOUND('',#3763,.T.);
#3140=FACE_OUTER_BOUND('',#3764,.T.);
#3141=FACE_OUTER_BOUND('',#3765,.T.);
#3142=FACE_OUTER_BOUND('',#3766,.T.);
#3143=FACE_OUTER_BOUND('',#3767,.T.);
#3144=FACE_OUTER_BOUND('',#3768,.T.);
#3145=FACE_OUTER_BOUND('',#3769,.T.);
#3146=FACE_OUTER_BOUND('',#3770,.T.);
#3147=FACE_OUTER_BOUND('',#3771,.T.);
#3148=FACE_OUTER_BOUND('',#3772,.T.);
#3149=FACE_OUTER_BOUND('',#3773,.T.);
#3150=FACE_OUTER_BOUND('',#3844,.T.);
#3151=FACE_OUTER_BOUND('',#3845,.T.);
#3152=FACE_OUTER_BOUND('',#3893,.T.);
#3153=FACE_OUTER_BOUND('',#3894,.T.);
#3154=FACE_OUTER_BOUND('',#3965,.T.);
#3155=FACE_OUTER_BOUND('',#3966,.T.);
#3156=FACE_OUTER_BOUND('',#3967,.T.);
#3157=FACE_OUTER_BOUND('',#3968,.T.);
#3158=FACE_OUTER_BOUND('',#3969,.T.);
#3159=FACE_OUTER_BOUND('',#3970,.T.);
#3160=FACE_OUTER_BOUND('',#3971,.T.);
#3161=FACE_OUTER_BOUND('',#3972,.T.);
#3162=FACE_OUTER_BOUND('',#3973,.T.);
#3163=FACE_OUTER_BOUND('',#3974,.T.);
#3164=FACE_OUTER_BOUND('',#3975,.T.);
#3165=FACE_OUTER_BOUND('',#3976,.T.);
#3166=FACE_OUTER_BOUND('',#3977,.T.);
#3167=FACE_OUTER_BOUND('',#3978,.T.);
#3168=FACE_OUTER_BOUND('',#3979,.T.);
#3169=FACE_OUTER_BOUND('',#3980,.T.);
#3170=FACE_OUTER_BOUND('',#3981,.T.);
#3171=FACE_OUTER_BOUND('',#3982,.T.);
#3172=FACE_OUTER_BOUND('',#3983,.T.);
#3173=FACE_OUTER_BOUND('',#3984,.T.);
#3174=FACE_OUTER_BOUND('',#3985,.T.);
#3175=FACE_OUTER_BOUND('',#3986,.T.);
#3176=FACE_OUTER_BOUND('',#3987,.T.);
#3177=FACE_OUTER_BOUND('',#3988,.T.);
#3178=FACE_OUTER_BOUND('',#3989,.T.);
#3179=FACE_OUTER_BOUND('',#3990,.T.);
#3180=FACE_OUTER_BOUND('',#3991,.T.);
#3181=FACE_OUTER_BOUND('',#3992,.T.);
#3182=FACE_OUTER_BOUND('',#3993,.T.);
#3183=FACE_OUTER_BOUND('',#3994,.T.);
#3184=FACE_OUTER_BOUND('',#3995,.T.);
#3185=FACE_OUTER_BOUND('',#3996,.T.);
#3186=FACE_OUTER_BOUND('',#3997,.T.);
#3187=FACE_OUTER_BOUND('',#3998,.T.);
#3188=FACE_OUTER_BOUND('',#3999,.T.);
#3189=FACE_OUTER_BOUND('',#4000,.T.);
#3190=FACE_OUTER_BOUND('',#4001,.T.);
#3191=FACE_OUTER_BOUND('',#4002,.T.);
#3192=FACE_OUTER_BOUND('',#4003,.T.);
#3193=FACE_OUTER_BOUND('',#4004,.T.);
#3194=FACE_OUTER_BOUND('',#4005,.T.);
#3195=FACE_OUTER_BOUND('',#4006,.T.);
#3196=FACE_OUTER_BOUND('',#4007,.T.);
#3197=FACE_OUTER_BOUND('',#4008,.T.);
#3198=FACE_OUTER_BOUND('',#4009,.T.);
#3199=FACE_OUTER_BOUND('',#4010,.T.);
#3200=FACE_OUTER_BOUND('',#4011,.T.);
#3201=FACE_OUTER_BOUND('',#4012,.T.);
#3202=FACE_OUTER_BOUND('',#4013,.T.);
#3203=FACE_OUTER_BOUND('',#4014,.T.);
#3204=FACE_OUTER_BOUND('',#4015,.T.);
#3205=FACE_OUTER_BOUND('',#4063,.T.);
#3206=FACE_OUTER_BOUND('',#4064,.T.);
#3207=FACE_OUTER_BOUND('',#4065,.T.);
#3208=FACE_OUTER_BOUND('',#4066,.T.);
#3209=FACE_OUTER_BOUND('',#4067,.T.);
#3210=FACE_OUTER_BOUND('',#4068,.T.);
#3211=FACE_OUTER_BOUND('',#4069,.T.);
#3212=FACE_OUTER_BOUND('',#4070,.T.);
#3213=FACE_OUTER_BOUND('',#4071,.T.);
#3214=FACE_OUTER_BOUND('',#4072,.T.);
#3215=FACE_OUTER_BOUND('',#4073,.T.);
#3216=FACE_OUTER_BOUND('',#4074,.T.);
#3217=FACE_OUTER_BOUND('',#4075,.T.);
#3218=FACE_OUTER_BOUND('',#4076,.T.);
#3219=FACE_OUTER_BOUND('',#4077,.T.);
#3220=FACE_OUTER_BOUND('',#4078,.T.);
#3221=FACE_OUTER_BOUND('',#4079,.T.);
#3222=FACE_OUTER_BOUND('',#4080,.T.);
#3223=FACE_OUTER_BOUND('',#4081,.T.);
#3224=FACE_OUTER_BOUND('',#4082,.T.);
#3225=FACE_OUTER_BOUND('',#4083,.T.);
#3226=FACE_OUTER_BOUND('',#4084,.T.);
#3227=FACE_OUTER_BOUND('',#4085,.T.);
#3228=FACE_OUTER_BOUND('',#4086,.T.);
#3229=FACE_OUTER_BOUND('',#4087,.T.);
#3230=FACE_OUTER_BOUND('',#4088,.T.);
#3231=FACE_OUTER_BOUND('',#4089,.T.);
#3232=FACE_OUTER_BOUND('',#4090,.T.);
#3233=FACE_OUTER_BOUND('',#4091,.T.);
#3234=FACE_OUTER_BOUND('',#4092,.T.);
#3235=FACE_OUTER_BOUND('',#4093,.T.);
#3236=FACE_OUTER_BOUND('',#4094,.T.);
#3237=FACE_OUTER_BOUND('',#4095,.T.);
#3238=FACE_OUTER_BOUND('',#4096,.T.);
#3239=FACE_OUTER_BOUND('',#4097,.T.);
#3240=FACE_OUTER_BOUND('',#4098,.T.);
#3241=FACE_OUTER_BOUND('',#4099,.T.);
#3242=FACE_OUTER_BOUND('',#4100,.T.);
#3243=FACE_OUTER_BOUND('',#4101,.T.);
#3244=FACE_OUTER_BOUND('',#4102,.T.);
#3245=FACE_OUTER_BOUND('',#4103,.T.);
#3246=FACE_OUTER_BOUND('',#4104,.T.);
#3247=FACE_OUTER_BOUND('',#4105,.T.);
#3248=FACE_OUTER_BOUND('',#4106,.T.);
#3249=FACE_OUTER_BOUND('',#4107,.T.);
#3250=FACE_OUTER_BOUND('',#4108,.T.);
#3251=FACE_OUTER_BOUND('',#4109,.T.);
#3252=FACE_OUTER_BOUND('',#4110,.T.);
#3253=FACE_OUTER_BOUND('',#4111,.T.);
#3254=FACE_OUTER_BOUND('',#4112,.T.);
#3255=FACE_OUTER_BOUND('',#4160,.T.);
#3256=FACE_OUTER_BOUND('',#4208,.T.);
#3257=FACE_OUTER_BOUND('',#4209,.T.);
#3258=FACE_OUTER_BOUND('',#4210,.T.);
#3259=FACE_OUTER_BOUND('',#4211,.T.);
#3260=FACE_OUTER_BOUND('',#4212,.T.);
#3261=FACE_OUTER_BOUND('',#4224,.T.);
#3262=FACE_OUTER_BOUND('',#4225,.T.);
#3263=FACE_OUTER_BOUND('',#4237,.T.);
#3264=FACE_OUTER_BOUND('',#4238,.T.);
#3265=FACE_OUTER_BOUND('',#4239,.T.);
#3266=FACE_OUTER_BOUND('',#4240,.T.);
#3267=FACE_OUTER_BOUND('',#4241,.T.);
#3268=FACE_OUTER_BOUND('',#4242,.T.);
#3269=FACE_OUTER_BOUND('',#4243,.T.);
#3270=FACE_OUTER_BOUND('',#4244,.T.);
#3271=FACE_OUTER_BOUND('',#4245,.T.);
#3272=FACE_OUTER_BOUND('',#4246,.T.);
#3273=FACE_OUTER_BOUND('',#4247,.T.);
#3274=FACE_OUTER_BOUND('',#4248,.T.);
#3275=FACE_OUTER_BOUND('',#4249,.T.);
#3276=FACE_OUTER_BOUND('',#4250,.T.);
#3277=FACE_OUTER_BOUND('',#4251,.T.);
#3278=FACE_OUTER_BOUND('',#4252,.T.);
#3279=FACE_OUTER_BOUND('',#4253,.T.);
#3280=FACE_OUTER_BOUND('',#4265,.T.);
#3281=FACE_OUTER_BOUND('',#4266,.T.);
#3282=FACE_OUTER_BOUND('',#4267,.T.);
#3283=FACE_OUTER_BOUND('',#4268,.T.);
#3284=FACE_OUTER_BOUND('',#4269,.T.);
#3285=FACE_OUTER_BOUND('',#4270,.T.);
#3286=FACE_OUTER_BOUND('',#4271,.T.);
#3287=FACE_OUTER_BOUND('',#4272,.T.);
#3288=FACE_OUTER_BOUND('',#4273,.T.);
#3289=FACE_OUTER_BOUND('',#4274,.T.);
#3290=FACE_OUTER_BOUND('',#4275,.T.);
#3291=FACE_OUTER_BOUND('',#4276,.T.);
#3292=FACE_OUTER_BOUND('',#4277,.T.);
#3293=FACE_OUTER_BOUND('',#4278,.T.);
#3294=FACE_OUTER_BOUND('',#4279,.T.);
#3295=FACE_OUTER_BOUND('',#4280,.T.);
#3296=FACE_OUTER_BOUND('',#4281,.T.);
#3297=FACE_OUTER_BOUND('',#4293,.T.);
#3298=FACE_OUTER_BOUND('',#4297,.T.);
#3299=FACE_OUTER_BOUND('',#4299,.T.);
#3300=FACE_OUTER_BOUND('',#4300,.T.);
#3301=FACE_OUTER_BOUND('',#4303,.T.);
#3302=FACE_OUTER_BOUND('',#4304,.T.);
#3303=FACE_OUTER_BOUND('',#4305,.T.);
#3304=FACE_OUTER_BOUND('',#4306,.T.);
#3305=FACE_OUTER_BOUND('',#4307,.T.);
#3306=FACE_OUTER_BOUND('',#4308,.T.);
#3307=FACE_OUTER_BOUND('',#4309,.T.);
#3308=FACE_OUTER_BOUND('',#4310,.T.);
#3309=FACE_OUTER_BOUND('',#4311,.T.);
#3310=FACE_OUTER_BOUND('',#4312,.T.);
#3311=FACE_OUTER_BOUND('',#4314,.T.);
#3312=FACE_OUTER_BOUND('',#4316,.T.);
#3313=FACE_OUTER_BOUND('',#4317,.T.);
#3314=FACE_OUTER_BOUND('',#4318,.T.);
#3315=FACE_OUTER_BOUND('',#4319,.T.);
#3316=FACE_OUTER_BOUND('',#4320,.T.);
#3317=FACE_OUTER_BOUND('',#4332,.T.);
#3318=FACE_OUTER_BOUND('',#4333,.T.);
#3319=FACE_OUTER_BOUND('',#4345,.T.);
#3320=FACE_OUTER_BOUND('',#4346,.T.);
#3321=FACE_OUTER_BOUND('',#4347,.T.);
#3322=FACE_OUTER_BOUND('',#4348,.T.);
#3323=FACE_OUTER_BOUND('',#4349,.T.);
#3324=FACE_OUTER_BOUND('',#4350,.T.);
#3325=FACE_OUTER_BOUND('',#4351,.T.);
#3326=FACE_OUTER_BOUND('',#4352,.T.);
#3327=FACE_OUTER_BOUND('',#4353,.T.);
#3328=FACE_OUTER_BOUND('',#4354,.T.);
#3329=FACE_OUTER_BOUND('',#4355,.T.);
#3330=FACE_OUTER_BOUND('',#4356,.T.);
#3331=FACE_OUTER_BOUND('',#4357,.T.);
#3332=FACE_OUTER_BOUND('',#4358,.T.);
#3333=FACE_OUTER_BOUND('',#4359,.T.);
#3334=FACE_OUTER_BOUND('',#4360,.T.);
#3335=FACE_OUTER_BOUND('',#4361,.T.);
#3336=FACE_OUTER_BOUND('',#4373,.T.);
#3337=FACE_OUTER_BOUND('',#4374,.T.);
#3338=FACE_OUTER_BOUND('',#4375,.T.);
#3339=FACE_OUTER_BOUND('',#4376,.T.);
#3340=FACE_OUTER_BOUND('',#4377,.T.);
#3341=FACE_OUTER_BOUND('',#4378,.T.);
#3342=FACE_OUTER_BOUND('',#4379,.T.);
#3343=FACE_OUTER_BOUND('',#4380,.T.);
#3344=FACE_OUTER_BOUND('',#4381,.T.);
#3345=FACE_OUTER_BOUND('',#4382,.T.);
#3346=FACE_OUTER_BOUND('',#4383,.T.);
#3347=FACE_OUTER_BOUND('',#4384,.T.);
#3348=FACE_OUTER_BOUND('',#4385,.T.);
#3349=FACE_OUTER_BOUND('',#4386,.T.);
#3350=FACE_OUTER_BOUND('',#4387,.T.);
#3351=FACE_OUTER_BOUND('',#4388,.T.);
#3352=FACE_OUTER_BOUND('',#4389,.T.);
#3353=FACE_OUTER_BOUND('',#4401,.T.);
#3354=FACE_OUTER_BOUND('',#4405,.T.);
#3355=FACE_OUTER_BOUND('',#4407,.T.);
#3356=FACE_OUTER_BOUND('',#4408,.T.);
#3357=FACE_OUTER_BOUND('',#4411,.T.);
#3358=FACE_OUTER_BOUND('',#4412,.T.);
#3359=FACE_OUTER_BOUND('',#4413,.T.);
#3360=FACE_OUTER_BOUND('',#4415,.T.);
#3361=FACE_OUTER_BOUND('',#4416,.T.);
#3362=FACE_OUTER_BOUND('',#4417,.T.);
#3363=FACE_OUTER_BOUND('',#4418,.T.);
#3364=FACE_OUTER_BOUND('',#4419,.T.);
#3365=FACE_OUTER_BOUND('',#4420,.T.);
#3366=FACE_OUTER_BOUND('',#4421,.T.);
#3367=FACE_OUTER_BOUND('',#4422,.T.);
#3368=FACE_OUTER_BOUND('',#4423,.T.);
#3369=FACE_OUTER_BOUND('',#4424,.T.);
#3370=FACE_OUTER_BOUND('',#4425,.T.);
#3371=FACE_OUTER_BOUND('',#4426,.T.);
#3372=FACE_OUTER_BOUND('',#4427,.T.);
#3373=FACE_OUTER_BOUND('',#4428,.T.);
#3374=FACE_OUTER_BOUND('',#4429,.T.);
#3375=FACE_OUTER_BOUND('',#4430,.T.);
#3376=FACE_OUTER_BOUND('',#4431,.T.);
#3377=FACE_OUTER_BOUND('',#4433,.T.);
#3378=FACE_OUTER_BOUND('',#4435,.T.);
#3379=FACE_OUTER_BOUND('',#4436,.T.);
#3380=FACE_OUTER_BOUND('',#4437,.T.);
#3381=FACE_OUTER_BOUND('',#4438,.T.);
#3382=FACE_OUTER_BOUND('',#4439,.T.);
#3383=FACE_OUTER_BOUND('',#4440,.T.);
#3384=FACE_OUTER_BOUND('',#4441,.T.);
#3385=FACE_OUTER_BOUND('',#4442,.T.);
#3386=FACE_OUTER_BOUND('',#4444,.T.);
#3387=FACE_OUTER_BOUND('',#4446,.T.);
#3388=FACE_OUTER_BOUND('',#4447,.T.);
#3389=FACE_OUTER_BOUND('',#4448,.T.);
#3390=FACE_OUTER_BOUND('',#4449,.T.);
#3391=FACE_OUTER_BOUND('',#4450,.T.);
#3392=FACE_OUTER_BOUND('',#4451,.T.);
#3393=FACE_OUTER_BOUND('',#4452,.T.);
#3394=FACE_OUTER_BOUND('',#4453,.T.);
#3395=FACE_OUTER_BOUND('',#4454,.T.);
#3396=FACE_OUTER_BOUND('',#4455,.T.);
#3397=FACE_OUTER_BOUND('',#4456,.T.);
#3398=FACE_OUTER_BOUND('',#4457,.T.);
#3399=FACE_OUTER_BOUND('',#4458,.T.);
#3400=FACE_OUTER_BOUND('',#4459,.T.);
#3401=FACE_OUTER_BOUND('',#4460,.T.);
#3402=FACE_OUTER_BOUND('',#4461,.T.);
#3403=FACE_OUTER_BOUND('',#4462,.T.);
#3404=FACE_OUTER_BOUND('',#4463,.T.);
#3405=FACE_OUTER_BOUND('',#4464,.T.);
#3406=FACE_OUTER_BOUND('',#4465,.T.);
#3407=FACE_OUTER_BOUND('',#4466,.T.);
#3408=FACE_OUTER_BOUND('',#4467,.T.);
#3409=FACE_OUTER_BOUND('',#4468,.T.);
#3410=FACE_OUTER_BOUND('',#4469,.T.);
#3411=FACE_OUTER_BOUND('',#4470,.T.);
#3412=FACE_OUTER_BOUND('',#4471,.T.);
#3413=FACE_OUTER_BOUND('',#4472,.T.);
#3414=FACE_OUTER_BOUND('',#4473,.T.);
#3415=FACE_OUTER_BOUND('',#4474,.T.);
#3416=FACE_OUTER_BOUND('',#4475,.T.);
#3417=FACE_OUTER_BOUND('',#4476,.T.);
#3418=FACE_OUTER_BOUND('',#4477,.T.);
#3419=FACE_OUTER_BOUND('',#4478,.T.);
#3420=FACE_OUTER_BOUND('',#4479,.T.);
#3421=FACE_OUTER_BOUND('',#4480,.T.);
#3422=FACE_OUTER_BOUND('',#4481,.T.);
#3423=FACE_OUTER_BOUND('',#4482,.T.);
#3424=FACE_OUTER_BOUND('',#4483,.T.);
#3425=FACE_OUTER_BOUND('',#4484,.T.);
#3426=FACE_OUTER_BOUND('',#4485,.T.);
#3427=FACE_OUTER_BOUND('',#4486,.T.);
#3428=FACE_OUTER_BOUND('',#4488,.T.);
#3429=FACE_OUTER_BOUND('',#4490,.T.);
#3430=FACE_OUTER_BOUND('',#4491,.T.);
#3431=FACE_OUTER_BOUND('',#4492,.T.);
#3432=FACE_OUTER_BOUND('',#4493,.T.);
#3433=FACE_OUTER_BOUND('',#4494,.T.);
#3434=FACE_OUTER_BOUND('',#4495,.T.);
#3435=FACE_OUTER_BOUND('',#4496,.T.);
#3436=FACE_OUTER_BOUND('',#4497,.T.);
#3437=FACE_OUTER_BOUND('',#4499,.T.);
#3438=EDGE_LOOP('',(#7712,#7713,#7714,#7715,#7716));
#3439=EDGE_LOOP('',(#7717,#7718,#7719,#7720,#7721,#7722));
#3440=EDGE_LOOP('',(#7723));
#3441=EDGE_LOOP('',(#7724,#7725,#7726,#7727,#7728));
#3442=EDGE_LOOP('',(#7729,#7730,#7731,#7732,#7733));
#3443=EDGE_LOOP('',(#7734,#7735,#7736,#7737,#7738,#7739));
#3444=EDGE_LOOP('',(#7740,#7741,#7742,#7743,#7744));
#3445=EDGE_LOOP('',(#7745));
#3446=EDGE_LOOP('',(#7746,#7747,#7748,#7749));
#3447=EDGE_LOOP('',(#7750,#7751,#7752,#7753,#7754));
#3448=EDGE_LOOP('',(#7755,#7756,#7757,#7758,#7759,#7760));
#3449=EDGE_LOOP('',(#7761));
#3450=EDGE_LOOP('',(#7762));
#3451=EDGE_LOOP('',(#7763,#7764,#7765,#7766,#7767));
#3452=EDGE_LOOP('',(#7768));
#3453=EDGE_LOOP('',(#7769));
#3454=EDGE_LOOP('',(#7770,#7771,#7772,#7773));
#3455=EDGE_LOOP('',(#7774));
#3456=EDGE_LOOP('',(#7775));
#3457=EDGE_LOOP('',(#7776));
#3458=EDGE_LOOP('',(#7777));
#3459=EDGE_LOOP('',(#7778));
#3460=EDGE_LOOP('',(#7779));
#3461=EDGE_LOOP('',(#7780,#7781,#7782,#7783));
#3462=EDGE_LOOP('',(#7784,#7785,#7786,#7787));
#3463=EDGE_LOOP('',(#7788));
#3464=EDGE_LOOP('',(#7789));
#3465=EDGE_LOOP('',(#7790,#7791,#7792,#7793));
#3466=EDGE_LOOP('',(#7794));
#3467=EDGE_LOOP('',(#7795));
#3468=EDGE_LOOP('',(#7796,#7797,#7798,#7799));
#3469=EDGE_LOOP('',(#7800,#7801,#7802,#7803));
#3470=EDGE_LOOP('',(#7804,#7805,#7806,#7807));
#3471=EDGE_LOOP('',(#7808));
#3472=EDGE_LOOP('',(#7809));
#3473=EDGE_LOOP('',(#7810,#7811,#7812,#7813));
#3474=EDGE_LOOP('',(#7814));
#3475=EDGE_LOOP('',(#7815));
#3476=EDGE_LOOP('',(#7816,#7817,#7818,#7819));
#3477=EDGE_LOOP('',(#7820,#7821,#7822,#7823));
#3478=EDGE_LOOP('',(#7824));
#3479=EDGE_LOOP('',(#7825));
#3480=EDGE_LOOP('',(#7826));
#3481=EDGE_LOOP('',(#7827));
#3482=EDGE_LOOP('',(#7828));
#3483=EDGE_LOOP('',(#7829));
#3484=EDGE_LOOP('',(#7830));
#3485=EDGE_LOOP('',(#7831));
#3486=EDGE_LOOP('',(#7832));
#3487=EDGE_LOOP('',(#7833));
#3488=EDGE_LOOP('',(#7834));
#3489=EDGE_LOOP('',(#7835,#7836,#7837,#7838,#7839,#7840,#7841,#7842,#7843,
#7844));
#3490=EDGE_LOOP('',(#7845,#7846,#7847,#7848));
#3491=EDGE_LOOP('',(#7849,#7850,#7851,#7852));
#3492=EDGE_LOOP('',(#7853,#7854,#7855,#7856));
#3493=EDGE_LOOP('',(#7857,#7858,#7859,#7860));
#3494=EDGE_LOOP('',(#7861,#7862,#7863,#7864));
#3495=EDGE_LOOP('',(#7865,#7866,#7867,#7868));
#3496=EDGE_LOOP('',(#7869,#7870,#7871,#7872));
#3497=EDGE_LOOP('',(#7873,#7874,#7875,#7876));
#3498=EDGE_LOOP('',(#7877,#7878,#7879,#7880));
#3499=EDGE_LOOP('',(#7881,#7882,#7883,#7884));
#3500=EDGE_LOOP('',(#7885,#7886,#7887,#7888));
#3501=EDGE_LOOP('',(#7889,#7890,#7891,#7892));
#3502=EDGE_LOOP('',(#7893,#7894,#7895,#7896));
#3503=EDGE_LOOP('',(#7897,#7898,#7899,#7900));
#3504=EDGE_LOOP('',(#7901,#7902,#7903,#7904));
#3505=EDGE_LOOP('',(#7905,#7906,#7907,#7908));
#3506=EDGE_LOOP('',(#7909,#7910,#7911,#7912));
#3507=EDGE_LOOP('',(#7913,#7914,#7915,#7916));
#3508=EDGE_LOOP('',(#7917,#7918,#7919,#7920));
#3509=EDGE_LOOP('',(#7921,#7922,#7923,#7924));
#3510=EDGE_LOOP('',(#7925,#7926,#7927,#7928));
#3511=EDGE_LOOP('',(#7929,#7930,#7931,#7932));
#3512=EDGE_LOOP('',(#7933,#7934,#7935,#7936));
#3513=EDGE_LOOP('',(#7937,#7938,#7939,#7940));
#3514=EDGE_LOOP('',(#7941,#7942,#7943,#7944));
#3515=EDGE_LOOP('',(#7945,#7946,#7947,#7948));
#3516=EDGE_LOOP('',(#7949,#7950,#7951,#7952));
#3517=EDGE_LOOP('',(#7953,#7954,#7955,#7956));
#3518=EDGE_LOOP('',(#7957,#7958,#7959,#7960));
#3519=EDGE_LOOP('',(#7961,#7962,#7963,#7964));
#3520=EDGE_LOOP('',(#7965,#7966,#7967,#7968));
#3521=EDGE_LOOP('',(#7969,#7970,#7971,#7972));
#3522=EDGE_LOOP('',(#7973,#7974,#7975,#7976));
#3523=EDGE_LOOP('',(#7977,#7978,#7979,#7980));
#3524=EDGE_LOOP('',(#7981,#7982,#7983,#7984));
#3525=EDGE_LOOP('',(#7985,#7986,#7987,#7988));
#3526=EDGE_LOOP('',(#7989));
#3527=EDGE_LOOP('',(#7990));
#3528=EDGE_LOOP('',(#7991));
#3529=EDGE_LOOP('',(#7992));
#3530=EDGE_LOOP('',(#7993));
#3531=EDGE_LOOP('',(#7994));
#3532=EDGE_LOOP('',(#7995));
#3533=EDGE_LOOP('',(#7996));
#3534=EDGE_LOOP('',(#7997));
#3535=EDGE_LOOP('',(#7998));
#3536=EDGE_LOOP('',(#7999));
#3537=EDGE_LOOP('',(#8000,#8001,#8002,#8003));
#3538=EDGE_LOOP('',(#8004));
#3539=EDGE_LOOP('',(#8005));
#3540=EDGE_LOOP('',(#8006));
#3541=EDGE_LOOP('',(#8007));
#3542=EDGE_LOOP('',(#8008));
#3543=EDGE_LOOP('',(#8009));
#3544=EDGE_LOOP('',(#8010));
#3545=EDGE_LOOP('',(#8011));
#3546=EDGE_LOOP('',(#8012));
#3547=EDGE_LOOP('',(#8013));
#3548=EDGE_LOOP('',(#8014));
#3549=EDGE_LOOP('',(#8015,#8016,#8017,#8018));
#3550=EDGE_LOOP('',(#8019,#8020,#8021,#8022));
#3551=EDGE_LOOP('',(#8023));
#3552=EDGE_LOOP('',(#8024));
#3553=EDGE_LOOP('',(#8025));
#3554=EDGE_LOOP('',(#8026));
#3555=EDGE_LOOP('',(#8027));
#3556=EDGE_LOOP('',(#8028));
#3557=EDGE_LOOP('',(#8029));
#3558=EDGE_LOOP('',(#8030));
#3559=EDGE_LOOP('',(#8031));
#3560=EDGE_LOOP('',(#8032));
#3561=EDGE_LOOP('',(#8033));
#3562=EDGE_LOOP('',(#8034,#8035,#8036,#8037));
#3563=EDGE_LOOP('',(#8038));
#3564=EDGE_LOOP('',(#8039));
#3565=EDGE_LOOP('',(#8040));
#3566=EDGE_LOOP('',(#8041));
#3567=EDGE_LOOP('',(#8042));
#3568=EDGE_LOOP('',(#8043));
#3569=EDGE_LOOP('',(#8044));
#3570=EDGE_LOOP('',(#8045));
#3571=EDGE_LOOP('',(#8046));
#3572=EDGE_LOOP('',(#8047));
#3573=EDGE_LOOP('',(#8048));
#3574=EDGE_LOOP('',(#8049,#8050,#8051,#8052));
#3575=EDGE_LOOP('',(#8053));
#3576=EDGE_LOOP('',(#8054));
#3577=EDGE_LOOP('',(#8055));
#3578=EDGE_LOOP('',(#8056));
#3579=EDGE_LOOP('',(#8057));
#3580=EDGE_LOOP('',(#8058));
#3581=EDGE_LOOP('',(#8059));
#3582=EDGE_LOOP('',(#8060));
#3583=EDGE_LOOP('',(#8061));
#3584=EDGE_LOOP('',(#8062));
#3585=EDGE_LOOP('',(#8063));
#3586=EDGE_LOOP('',(#8064,#8065,#8066,#8067,#8068,#8069,#8070,#8071,#8072,
#8073));
#3587=EDGE_LOOP('',(#8074,#8075,#8076,#8077,#8078,#8079));
#3588=EDGE_LOOP('',(#8080));
#3589=EDGE_LOOP('',(#8081,#8082,#8083,#8084));
#3590=EDGE_LOOP('',(#8085,#8086,#8087,#8088));
#3591=EDGE_LOOP('',(#8089,#8090,#8091,#8092));
#3592=EDGE_LOOP('',(#8093,#8094,#8095,#8096));
#3593=EDGE_LOOP('',(#8097,#8098,#8099,#8100));
#3594=EDGE_LOOP('',(#8101,#8102,#8103,#8104));
#3595=EDGE_LOOP('',(#8105,#8106,#8107,#8108,#8109,#8110));
#3596=EDGE_LOOP('',(#8111,#8112,#8113,#8114));
#3597=EDGE_LOOP('',(#8115));
#3598=EDGE_LOOP('',(#8116,#8117,#8118,#8119));
#3599=EDGE_LOOP('',(#8120,#8121,#8122,#8123));
#3600=EDGE_LOOP('',(#8124,#8125,#8126,#8127));
#3601=EDGE_LOOP('',(#8128,#8129,#8130,#8131));
#3602=EDGE_LOOP('',(#8132,#8133,#8134,#8135));
#3603=EDGE_LOOP('',(#8136,#8137,#8138,#8139));
#3604=EDGE_LOOP('',(#8140,#8141,#8142,#8143));
#3605=EDGE_LOOP('',(#8144,#8145,#8146,#8147));
#3606=EDGE_LOOP('',(#8148,#8149,#8150,#8151));
#3607=EDGE_LOOP('',(#8152,#8153,#8154,#8155));
#3608=EDGE_LOOP('',(#8156,#8157,#8158,#8159));
#3609=EDGE_LOOP('',(#8160,#8161,#8162,#8163));
#3610=EDGE_LOOP('',(#8164,#8165,#8166,#8167));
#3611=EDGE_LOOP('',(#8168,#8169,#8170,#8171));
#3612=EDGE_LOOP('',(#8172,#8173,#8174,#8175));
#3613=EDGE_LOOP('',(#8176,#8177,#8178,#8179));
#3614=EDGE_LOOP('',(#8180,#8181,#8182,#8183));
#3615=EDGE_LOOP('',(#8184,#8185,#8186,#8187));
#3616=EDGE_LOOP('',(#8188,#8189,#8190,#8191));
#3617=EDGE_LOOP('',(#8192,#8193,#8194,#8195));
#3618=EDGE_LOOP('',(#8196,#8197,#8198,#8199));
#3619=EDGE_LOOP('',(#8200,#8201,#8202,#8203));
#3620=EDGE_LOOP('',(#8204,#8205,#8206,#8207));
#3621=EDGE_LOOP('',(#8208,#8209,#8210,#8211));
#3622=EDGE_LOOP('',(#8212,#8213,#8214,#8215));
#3623=EDGE_LOOP('',(#8216,#8217,#8218,#8219));
#3624=EDGE_LOOP('',(#8220,#8221,#8222,#8223));
#3625=EDGE_LOOP('',(#8224,#8225,#8226,#8227));
#3626=EDGE_LOOP('',(#8228,#8229,#8230,#8231));
#3627=EDGE_LOOP('',(#8232,#8233,#8234,#8235));
#3628=EDGE_LOOP('',(#8236,#8237,#8238,#8239));
#3629=EDGE_LOOP('',(#8240,#8241,#8242,#8243));
#3630=EDGE_LOOP('',(#8244,#8245,#8246,#8247));
#3631=EDGE_LOOP('',(#8248,#8249,#8250,#8251));
#3632=EDGE_LOOP('',(#8252,#8253,#8254,#8255));
#3633=EDGE_LOOP('',(#8256,#8257,#8258,#8259));
#3634=EDGE_LOOP('',(#8260,#8261,#8262,#8263));
#3635=EDGE_LOOP('',(#8264,#8265,#8266,#8267));
#3636=EDGE_LOOP('',(#8268,#8269,#8270,#8271));
#3637=EDGE_LOOP('',(#8272,#8273,#8274,#8275));
#3638=EDGE_LOOP('',(#8276,#8277,#8278,#8279,#8280,#8281,#8282,#8283,#8284,
#8285,#8286,#8287,#8288,#8289,#8290,#8291,#8292,#8293,#8294,#8295,#8296,
#8297,#8298,#8299,#8300,#8301,#8302,#8303,#8304,#8305));
#3639=EDGE_LOOP('',(#8306,#8307,#8308,#8309,#8310,#8311,#8312,#8313,#8314,
#8315));
#3640=EDGE_LOOP('',(#8316,#8317,#8318,#8319,#8320,#8321,#8322,#8323,#8324,
#8325,#8326,#8327,#8328,#8329,#8330,#8331,#8332,#8333,#8334,#8335,#8336,
#8337,#8338,#8339,#8340,#8341,#8342,#8343,#8344,#8345));
#3641=EDGE_LOOP('',(#8346,#8347,#8348,#8349,#8350,#8351,#8352,#8353,#8354,
#8355));
#3642=EDGE_LOOP('',(#8356,#8357,#8358,#8359));
#3643=EDGE_LOOP('',(#8360,#8361,#8362,#8363));
#3644=EDGE_LOOP('',(#8364,#8365,#8366,#8367));
#3645=EDGE_LOOP('',(#8368,#8369,#8370,#8371));
#3646=EDGE_LOOP('',(#8372,#8373,#8374,#8375));
#3647=EDGE_LOOP('',(#8376,#8377,#8378,#8379));
#3648=EDGE_LOOP('',(#8380,#8381,#8382,#8383));
#3649=EDGE_LOOP('',(#8384,#8385,#8386,#8387));
#3650=EDGE_LOOP('',(#8388,#8389,#8390,#8391));
#3651=EDGE_LOOP('',(#8392,#8393,#8394,#8395));
#3652=EDGE_LOOP('',(#8396,#8397,#8398,#8399));
#3653=EDGE_LOOP('',(#8400,#8401,#8402,#8403));
#3654=EDGE_LOOP('',(#8404,#8405,#8406,#8407));
#3655=EDGE_LOOP('',(#8408,#8409,#8410,#8411));
#3656=EDGE_LOOP('',(#8412,#8413,#8414,#8415));
#3657=EDGE_LOOP('',(#8416,#8417,#8418,#8419));
#3658=EDGE_LOOP('',(#8420,#8421,#8422,#8423));
#3659=EDGE_LOOP('',(#8424,#8425,#8426,#8427));
#3660=EDGE_LOOP('',(#8428,#8429,#8430,#8431));
#3661=EDGE_LOOP('',(#8432,#8433,#8434,#8435));
#3662=EDGE_LOOP('',(#8436,#8437,#8438,#8439));
#3663=EDGE_LOOP('',(#8440,#8441,#8442,#8443));
#3664=EDGE_LOOP('',(#8444,#8445,#8446,#8447));
#3665=EDGE_LOOP('',(#8448,#8449,#8450,#8451));
#3666=EDGE_LOOP('',(#8452,#8453,#8454,#8455));
#3667=EDGE_LOOP('',(#8456,#8457,#8458,#8459));
#3668=EDGE_LOOP('',(#8460,#8461,#8462,#8463));
#3669=EDGE_LOOP('',(#8464,#8465,#8466,#8467));
#3670=EDGE_LOOP('',(#8468,#8469,#8470,#8471));
#3671=EDGE_LOOP('',(#8472,#8473,#8474,#8475));
#3672=EDGE_LOOP('',(#8476,#8477,#8478,#8479));
#3673=EDGE_LOOP('',(#8480,#8481,#8482,#8483));
#3674=EDGE_LOOP('',(#8484,#8485,#8486,#8487));
#3675=EDGE_LOOP('',(#8488,#8489,#8490,#8491));
#3676=EDGE_LOOP('',(#8492,#8493,#8494,#8495));
#3677=EDGE_LOOP('',(#8496,#8497,#8498,#8499));
#3678=EDGE_LOOP('',(#8500,#8501,#8502,#8503));
#3679=EDGE_LOOP('',(#8504,#8505,#8506,#8507));
#3680=EDGE_LOOP('',(#8508,#8509,#8510,#8511));
#3681=EDGE_LOOP('',(#8512,#8513,#8514,#8515));
#3682=EDGE_LOOP('',(#8516,#8517,#8518,#8519));
#3683=EDGE_LOOP('',(#8520,#8521,#8522,#8523));
#3684=EDGE_LOOP('',(#8524,#8525,#8526,#8527));
#3685=EDGE_LOOP('',(#8528,#8529,#8530,#8531));
#3686=EDGE_LOOP('',(#8532,#8533,#8534,#8535));
#3687=EDGE_LOOP('',(#8536,#8537,#8538,#8539));
#3688=EDGE_LOOP('',(#8540,#8541,#8542,#8543));
#3689=EDGE_LOOP('',(#8544,#8545,#8546,#8547));
#3690=EDGE_LOOP('',(#8548,#8549,#8550,#8551));
#3691=EDGE_LOOP('',(#8552,#8553,#8554,#8555));
#3692=EDGE_LOOP('',(#8556,#8557,#8558,#8559));
#3693=EDGE_LOOP('',(#8560,#8561,#8562,#8563));
#3694=EDGE_LOOP('',(#8564,#8565,#8566,#8567));
#3695=EDGE_LOOP('',(#8568,#8569,#8570,#8571));
#3696=EDGE_LOOP('',(#8572,#8573,#8574,#8575));
#3697=EDGE_LOOP('',(#8576,#8577,#8578,#8579));
#3698=EDGE_LOOP('',(#8580,#8581,#8582,#8583));
#3699=EDGE_LOOP('',(#8584,#8585,#8586,#8587));
#3700=EDGE_LOOP('',(#8588,#8589,#8590,#8591));
#3701=EDGE_LOOP('',(#8592,#8593,#8594,#8595));
#3702=EDGE_LOOP('',(#8596,#8597,#8598,#8599));
#3703=EDGE_LOOP('',(#8600,#8601,#8602,#8603));
#3704=EDGE_LOOP('',(#8604,#8605,#8606,#8607));
#3705=EDGE_LOOP('',(#8608,#8609,#8610,#8611));
#3706=EDGE_LOOP('',(#8612,#8613,#8614,#8615));
#3707=EDGE_LOOP('',(#8616,#8617,#8618,#8619));
#3708=EDGE_LOOP('',(#8620,#8621,#8622,#8623));
#3709=EDGE_LOOP('',(#8624,#8625,#8626,#8627));
#3710=EDGE_LOOP('',(#8628,#8629,#8630,#8631));
#3711=EDGE_LOOP('',(#8632,#8633,#8634,#8635));
#3712=EDGE_LOOP('',(#8636,#8637,#8638,#8639));
#3713=EDGE_LOOP('',(#8640,#8641,#8642,#8643));
#3714=EDGE_LOOP('',(#8644,#8645,#8646,#8647));
#3715=EDGE_LOOP('',(#8648,#8649,#8650,#8651));
#3716=EDGE_LOOP('',(#8652,#8653,#8654,#8655));
#3717=EDGE_LOOP('',(#8656,#8657,#8658,#8659));
#3718=EDGE_LOOP('',(#8660,#8661,#8662,#8663));
#3719=EDGE_LOOP('',(#8664,#8665,#8666,#8667));
#3720=EDGE_LOOP('',(#8668,#8669,#8670,#8671));
#3721=EDGE_LOOP('',(#8672,#8673,#8674,#8675));
#3722=EDGE_LOOP('',(#8676,#8677,#8678,#8679));
#3723=EDGE_LOOP('',(#8680,#8681,#8682,#8683));
#3724=EDGE_LOOP('',(#8684,#8685,#8686,#8687));
#3725=EDGE_LOOP('',(#8688,#8689,#8690,#8691));
#3726=EDGE_LOOP('',(#8692,#8693,#8694,#8695));
#3727=EDGE_LOOP('',(#8696,#8697,#8698,#8699));
#3728=EDGE_LOOP('',(#8700,#8701,#8702,#8703));
#3729=EDGE_LOOP('',(#8704,#8705,#8706,#8707));
#3730=EDGE_LOOP('',(#8708,#8709,#8710,#8711));
#3731=EDGE_LOOP('',(#8712,#8713,#8714,#8715));
#3732=EDGE_LOOP('',(#8716,#8717,#8718,#8719));
#3733=EDGE_LOOP('',(#8720,#8721,#8722,#8723));
#3734=EDGE_LOOP('',(#8724,#8725,#8726,#8727));
#3735=EDGE_LOOP('',(#8728,#8729,#8730,#8731));
#3736=EDGE_LOOP('',(#8732,#8733,#8734,#8735));
#3737=EDGE_LOOP('',(#8736,#8737,#8738,#8739));
#3738=EDGE_LOOP('',(#8740,#8741,#8742,#8743));
#3739=EDGE_LOOP('',(#8744,#8745,#8746,#8747));
#3740=EDGE_LOOP('',(#8748,#8749,#8750,#8751));
#3741=EDGE_LOOP('',(#8752,#8753,#8754,#8755));
#3742=EDGE_LOOP('',(#8756,#8757,#8758,#8759));
#3743=EDGE_LOOP('',(#8760,#8761,#8762,#8763));
#3744=EDGE_LOOP('',(#8764,#8765,#8766,#8767));
#3745=EDGE_LOOP('',(#8768,#8769,#8770,#8771));
#3746=EDGE_LOOP('',(#8772,#8773,#8774,#8775));
#3747=EDGE_LOOP('',(#8776,#8777,#8778,#8779));
#3748=EDGE_LOOP('',(#8780,#8781,#8782,#8783));
#3749=EDGE_LOOP('',(#8784,#8785,#8786,#8787));
#3750=EDGE_LOOP('',(#8788,#8789,#8790,#8791));
#3751=EDGE_LOOP('',(#8792,#8793,#8794,#8795));
#3752=EDGE_LOOP('',(#8796,#8797,#8798,#8799));
#3753=EDGE_LOOP('',(#8800,#8801,#8802,#8803));
#3754=EDGE_LOOP('',(#8804,#8805,#8806,#8807));
#3755=EDGE_LOOP('',(#8808,#8809,#8810,#8811));
#3756=EDGE_LOOP('',(#8812,#8813,#8814,#8815));
#3757=EDGE_LOOP('',(#8816,#8817,#8818,#8819));
#3758=EDGE_LOOP('',(#8820,#8821,#8822,#8823));
#3759=EDGE_LOOP('',(#8824,#8825,#8826,#8827));
#3760=EDGE_LOOP('',(#8828,#8829,#8830,#8831));
#3761=EDGE_LOOP('',(#8832,#8833,#8834,#8835));
#3762=EDGE_LOOP('',(#8836,#8837,#8838,#8839));
#3763=EDGE_LOOP('',(#8840,#8841,#8842,#8843));
#3764=EDGE_LOOP('',(#8844,#8845,#8846,#8847));
#3765=EDGE_LOOP('',(#8848,#8849,#8850,#8851));
#3766=EDGE_LOOP('',(#8852,#8853,#8854,#8855));
#3767=EDGE_LOOP('',(#8856,#8857,#8858,#8859));
#3768=EDGE_LOOP('',(#8860,#8861,#8862,#8863));
#3769=EDGE_LOOP('',(#8864,#8865,#8866,#8867));
#3770=EDGE_LOOP('',(#8868,#8869,#8870,#8871));
#3771=EDGE_LOOP('',(#8872,#8873,#8874,#8875));
#3772=EDGE_LOOP('',(#8876,#8877,#8878,#8879));
#3773=EDGE_LOOP('',(#8880,#8881,#8882,#8883));
#3774=EDGE_LOOP('',(#8884));
#3775=EDGE_LOOP('',(#8885));
#3776=EDGE_LOOP('',(#8886,#8887,#8888,#8889));
#3777=EDGE_LOOP('',(#8890,#8891,#8892,#8893));
#3778=EDGE_LOOP('',(#8894));
#3779=EDGE_LOOP('',(#8895));
#3780=EDGE_LOOP('',(#8896));
#3781=EDGE_LOOP('',(#8897,#8898,#8899,#8900));
#3782=EDGE_LOOP('',(#8901,#8902,#8903,#8904));
#3783=EDGE_LOOP('',(#8905));
#3784=EDGE_LOOP('',(#8906));
#3785=EDGE_LOOP('',(#8907));
#3786=EDGE_LOOP('',(#8908));
#3787=EDGE_LOOP('',(#8909));
#3788=EDGE_LOOP('',(#8910,#8911,#8912,#8913));
#3789=EDGE_LOOP('',(#8914,#8915,#8916,#8917));
#3790=EDGE_LOOP('',(#8918));
#3791=EDGE_LOOP('',(#8919));
#3792=EDGE_LOOP('',(#8920));
#3793=EDGE_LOOP('',(#8921));
#3794=EDGE_LOOP('',(#8922));
#3795=EDGE_LOOP('',(#8923,#8924,#8925,#8926));
#3796=EDGE_LOOP('',(#8927,#8928,#8929,#8930));
#3797=EDGE_LOOP('',(#8931));
#3798=EDGE_LOOP('',(#8932));
#3799=EDGE_LOOP('',(#8933));
#3800=EDGE_LOOP('',(#8934));
#3801=EDGE_LOOP('',(#8935));
#3802=EDGE_LOOP('',(#8936,#8937,#8938,#8939));
#3803=EDGE_LOOP('',(#8940,#8941,#8942,#8943));
#3804=EDGE_LOOP('',(#8944));
#3805=EDGE_LOOP('',(#8945));
#3806=EDGE_LOOP('',(#8946));
#3807=EDGE_LOOP('',(#8947));
#3808=EDGE_LOOP('',(#8948));
#3809=EDGE_LOOP('',(#8949,#8950,#8951,#8952));
#3810=EDGE_LOOP('',(#8953,#8954,#8955,#8956));
#3811=EDGE_LOOP('',(#8957));
#3812=EDGE_LOOP('',(#8958));
#3813=EDGE_LOOP('',(#8959));
#3814=EDGE_LOOP('',(#8960));
#3815=EDGE_LOOP('',(#8961));
#3816=EDGE_LOOP('',(#8962,#8963,#8964,#8965));
#3817=EDGE_LOOP('',(#8966,#8967,#8968,#8969));
#3818=EDGE_LOOP('',(#8970));
#3819=EDGE_LOOP('',(#8971));
#3820=EDGE_LOOP('',(#8972));
#3821=EDGE_LOOP('',(#8973));
#3822=EDGE_LOOP('',(#8974));
#3823=EDGE_LOOP('',(#8975,#8976,#8977,#8978));
#3824=EDGE_LOOP('',(#8979,#8980,#8981,#8982));
#3825=EDGE_LOOP('',(#8983));
#3826=EDGE_LOOP('',(#8984));
#3827=EDGE_LOOP('',(#8985));
#3828=EDGE_LOOP('',(#8986));
#3829=EDGE_LOOP('',(#8987));
#3830=EDGE_LOOP('',(#8988,#8989,#8990,#8991));
#3831=EDGE_LOOP('',(#8992,#8993,#8994,#8995));
#3832=EDGE_LOOP('',(#8996));
#3833=EDGE_LOOP('',(#8997));
#3834=EDGE_LOOP('',(#8998));
#3835=EDGE_LOOP('',(#8999));
#3836=EDGE_LOOP('',(#9000));
#3837=EDGE_LOOP('',(#9001,#9002,#9003,#9004));
#3838=EDGE_LOOP('',(#9005,#9006,#9007,#9008));
#3839=EDGE_LOOP('',(#9009));
#3840=EDGE_LOOP('',(#9010));
#3841=EDGE_LOOP('',(#9011));
#3842=EDGE_LOOP('',(#9012));
#3843=EDGE_LOOP('',(#9013));
#3844=EDGE_LOOP('',(#9014,#9015,#9016,#9017));
#3845=EDGE_LOOP('',(#9018,#9019,#9020,#9021));
#3846=EDGE_LOOP('',(#9022));
#3847=EDGE_LOOP('',(#9023));
#3848=EDGE_LOOP('',(#9024));
#3849=EDGE_LOOP('',(#9025));
#3850=EDGE_LOOP('',(#9026));
#3851=EDGE_LOOP('',(#9027));
#3852=EDGE_LOOP('',(#9028));
#3853=EDGE_LOOP('',(#9029));
#3854=EDGE_LOOP('',(#9030));
#3855=EDGE_LOOP('',(#9031));
#3856=EDGE_LOOP('',(#9032));
#3857=EDGE_LOOP('',(#9033));
#3858=EDGE_LOOP('',(#9034));
#3859=EDGE_LOOP('',(#9035));
#3860=EDGE_LOOP('',(#9036));
#3861=EDGE_LOOP('',(#9037));
#3862=EDGE_LOOP('',(#9038));
#3863=EDGE_LOOP('',(#9039));
#3864=EDGE_LOOP('',(#9040));
#3865=EDGE_LOOP('',(#9041));
#3866=EDGE_LOOP('',(#9042));
#3867=EDGE_LOOP('',(#9043));
#3868=EDGE_LOOP('',(#9044));
#3869=EDGE_LOOP('',(#9045));
#3870=EDGE_LOOP('',(#9046));
#3871=EDGE_LOOP('',(#9047));
#3872=EDGE_LOOP('',(#9048));
#3873=EDGE_LOOP('',(#9049));
#3874=EDGE_LOOP('',(#9050));
#3875=EDGE_LOOP('',(#9051));
#3876=EDGE_LOOP('',(#9052));
#3877=EDGE_LOOP('',(#9053));
#3878=EDGE_LOOP('',(#9054));
#3879=EDGE_LOOP('',(#9055));
#3880=EDGE_LOOP('',(#9056));
#3881=EDGE_LOOP('',(#9057));
#3882=EDGE_LOOP('',(#9058));
#3883=EDGE_LOOP('',(#9059));
#3884=EDGE_LOOP('',(#9060));
#3885=EDGE_LOOP('',(#9061));
#3886=EDGE_LOOP('',(#9062));
#3887=EDGE_LOOP('',(#9063));
#3888=EDGE_LOOP('',(#9064));
#3889=EDGE_LOOP('',(#9065));
#3890=EDGE_LOOP('',(#9066));
#3891=EDGE_LOOP('',(#9067));
#3892=EDGE_LOOP('',(#9068));
#3893=EDGE_LOOP('',(#9069,#9070,#9071,#9072));
#3894=EDGE_LOOP('',(#9073,#9074,#9075,#9076));
#3895=EDGE_LOOP('',(#9077));
#3896=EDGE_LOOP('',(#9078));
#3897=EDGE_LOOP('',(#9079,#9080,#9081,#9082));
#3898=EDGE_LOOP('',(#9083,#9084,#9085,#9086));
#3899=EDGE_LOOP('',(#9087));
#3900=EDGE_LOOP('',(#9088));
#3901=EDGE_LOOP('',(#9089));
#3902=EDGE_LOOP('',(#9090,#9091,#9092,#9093));
#3903=EDGE_LOOP('',(#9094,#9095,#9096,#9097));
#3904=EDGE_LOOP('',(#9098));
#3905=EDGE_LOOP('',(#9099));
#3906=EDGE_LOOP('',(#9100));
#3907=EDGE_LOOP('',(#9101));
#3908=EDGE_LOOP('',(#9102));
#3909=EDGE_LOOP('',(#9103,#9104,#9105,#9106));
#3910=EDGE_LOOP('',(#9107,#9108,#9109,#9110));
#3911=EDGE_LOOP('',(#9111));
#3912=EDGE_LOOP('',(#9112));
#3913=EDGE_LOOP('',(#9113));
#3914=EDGE_LOOP('',(#9114));
#3915=EDGE_LOOP('',(#9115));
#3916=EDGE_LOOP('',(#9116,#9117,#9118,#9119));
#3917=EDGE_LOOP('',(#9120,#9121,#9122,#9123));
#3918=EDGE_LOOP('',(#9124));
#3919=EDGE_LOOP('',(#9125));
#3920=EDGE_LOOP('',(#9126));
#3921=EDGE_LOOP('',(#9127));
#3922=EDGE_LOOP('',(#9128));
#3923=EDGE_LOOP('',(#9129,#9130,#9131,#9132));
#3924=EDGE_LOOP('',(#9133,#9134,#9135,#9136));
#3925=EDGE_LOOP('',(#9137));
#3926=EDGE_LOOP('',(#9138));
#3927=EDGE_LOOP('',(#9139));
#3928=EDGE_LOOP('',(#9140));
#3929=EDGE_LOOP('',(#9141));
#3930=EDGE_LOOP('',(#9142,#9143,#9144,#9145));
#3931=EDGE_LOOP('',(#9146,#9147,#9148,#9149));
#3932=EDGE_LOOP('',(#9150));
#3933=EDGE_LOOP('',(#9151));
#3934=EDGE_LOOP('',(#9152));
#3935=EDGE_LOOP('',(#9153));
#3936=EDGE_LOOP('',(#9154));
#3937=EDGE_LOOP('',(#9155,#9156,#9157,#9158));
#3938=EDGE_LOOP('',(#9159,#9160,#9161,#9162));
#3939=EDGE_LOOP('',(#9163));
#3940=EDGE_LOOP('',(#9164));
#3941=EDGE_LOOP('',(#9165));
#3942=EDGE_LOOP('',(#9166));
#3943=EDGE_LOOP('',(#9167));
#3944=EDGE_LOOP('',(#9168,#9169,#9170,#9171));
#3945=EDGE_LOOP('',(#9172,#9173,#9174,#9175));
#3946=EDGE_LOOP('',(#9176));
#3947=EDGE_LOOP('',(#9177));
#3948=EDGE_LOOP('',(#9178));
#3949=EDGE_LOOP('',(#9179));
#3950=EDGE_LOOP('',(#9180));
#3951=EDGE_LOOP('',(#9181,#9182,#9183,#9184));
#3952=EDGE_LOOP('',(#9185,#9186,#9187,#9188));
#3953=EDGE_LOOP('',(#9189));
#3954=EDGE_LOOP('',(#9190));
#3955=EDGE_LOOP('',(#9191));
#3956=EDGE_LOOP('',(#9192));
#3957=EDGE_LOOP('',(#9193));
#3958=EDGE_LOOP('',(#9194,#9195,#9196,#9197));
#3959=EDGE_LOOP('',(#9198,#9199,#9200,#9201));
#3960=EDGE_LOOP('',(#9202));
#3961=EDGE_LOOP('',(#9203));
#3962=EDGE_LOOP('',(#9204));
#3963=EDGE_LOOP('',(#9205));
#3964=EDGE_LOOP('',(#9206));
#3965=EDGE_LOOP('',(#9207,#9208,#9209,#9210,#9211,#9212,#9213,#9214,#9215,
#9216,#9217,#9218));
#3966=EDGE_LOOP('',(#9219,#9220,#9221,#9222));
#3967=EDGE_LOOP('',(#9223,#9224,#9225,#9226));
#3968=EDGE_LOOP('',(#9227,#9228,#9229,#9230));
#3969=EDGE_LOOP('',(#9231,#9232,#9233,#9234));
#3970=EDGE_LOOP('',(#9235,#9236,#9237,#9238));
#3971=EDGE_LOOP('',(#9239,#9240,#9241,#9242));
#3972=EDGE_LOOP('',(#9243,#9244,#9245,#9246));
#3973=EDGE_LOOP('',(#9247,#9248,#9249,#9250));
#3974=EDGE_LOOP('',(#9251,#9252,#9253,#9254));
#3975=EDGE_LOOP('',(#9255,#9256,#9257,#9258));
#3976=EDGE_LOOP('',(#9259,#9260,#9261,#9262));
#3977=EDGE_LOOP('',(#9263,#9264,#9265,#9266));
#3978=EDGE_LOOP('',(#9267,#9268,#9269,#9270));
#3979=EDGE_LOOP('',(#9271,#9272,#9273,#9274));
#3980=EDGE_LOOP('',(#9275,#9276,#9277,#9278));
#3981=EDGE_LOOP('',(#9279,#9280,#9281,#9282));
#3982=EDGE_LOOP('',(#9283,#9284,#9285,#9286));
#3983=EDGE_LOOP('',(#9287,#9288,#9289,#9290));
#3984=EDGE_LOOP('',(#9291,#9292,#9293,#9294));
#3985=EDGE_LOOP('',(#9295,#9296,#9297,#9298));
#3986=EDGE_LOOP('',(#9299,#9300,#9301,#9302));
#3987=EDGE_LOOP('',(#9303,#9304,#9305,#9306));
#3988=EDGE_LOOP('',(#9307,#9308,#9309,#9310));
#3989=EDGE_LOOP('',(#9311,#9312,#9313,#9314));
#3990=EDGE_LOOP('',(#9315,#9316,#9317,#9318));
#3991=EDGE_LOOP('',(#9319,#9320,#9321,#9322));
#3992=EDGE_LOOP('',(#9323,#9324,#9325,#9326));
#3993=EDGE_LOOP('',(#9327,#9328,#9329,#9330));
#3994=EDGE_LOOP('',(#9331,#9332,#9333,#9334));
#3995=EDGE_LOOP('',(#9335,#9336,#9337,#9338));
#3996=EDGE_LOOP('',(#9339,#9340,#9341,#9342));
#3997=EDGE_LOOP('',(#9343,#9344,#9345,#9346));
#3998=EDGE_LOOP('',(#9347,#9348,#9349,#9350));
#3999=EDGE_LOOP('',(#9351,#9352,#9353,#9354));
#4000=EDGE_LOOP('',(#9355,#9356,#9357,#9358));
#4001=EDGE_LOOP('',(#9359,#9360,#9361,#9362));
#4002=EDGE_LOOP('',(#9363,#9364,#9365,#9366));
#4003=EDGE_LOOP('',(#9367,#9368,#9369,#9370));
#4004=EDGE_LOOP('',(#9371,#9372,#9373,#9374));
#4005=EDGE_LOOP('',(#9375,#9376,#9377,#9378));
#4006=EDGE_LOOP('',(#9379,#9380,#9381,#9382));
#4007=EDGE_LOOP('',(#9383,#9384,#9385,#9386));
#4008=EDGE_LOOP('',(#9387,#9388,#9389,#9390));
#4009=EDGE_LOOP('',(#9391,#9392,#9393,#9394));
#4010=EDGE_LOOP('',(#9395,#9396,#9397,#9398));
#4011=EDGE_LOOP('',(#9399,#9400,#9401,#9402));
#4012=EDGE_LOOP('',(#9403,#9404,#9405,#9406));
#4013=EDGE_LOOP('',(#9407,#9408,#9409,#9410));
#4014=EDGE_LOOP('',(#9411,#9412,#9413,#9414));
#4015=EDGE_LOOP('',(#9415,#9416,#9417,#9418));
#4016=EDGE_LOOP('',(#9419));
#4017=EDGE_LOOP('',(#9420));
#4018=EDGE_LOOP('',(#9421));
#4019=EDGE_LOOP('',(#9422));
#4020=EDGE_LOOP('',(#9423));
#4021=EDGE_LOOP('',(#9424));
#4022=EDGE_LOOP('',(#9425));
#4023=EDGE_LOOP('',(#9426));
#4024=EDGE_LOOP('',(#9427));
#4025=EDGE_LOOP('',(#9428));
#4026=EDGE_LOOP('',(#9429));
#4027=EDGE_LOOP('',(#9430));
#4028=EDGE_LOOP('',(#9431));
#4029=EDGE_LOOP('',(#9432));
#4030=EDGE_LOOP('',(#9433));
#4031=EDGE_LOOP('',(#9434));
#4032=EDGE_LOOP('',(#9435));
#4033=EDGE_LOOP('',(#9436));
#4034=EDGE_LOOP('',(#9437));
#4035=EDGE_LOOP('',(#9438));
#4036=EDGE_LOOP('',(#9439));
#4037=EDGE_LOOP('',(#9440));
#4038=EDGE_LOOP('',(#9441));
#4039=EDGE_LOOP('',(#9442));
#4040=EDGE_LOOP('',(#9443));
#4041=EDGE_LOOP('',(#9444));
#4042=EDGE_LOOP('',(#9445));
#4043=EDGE_LOOP('',(#9446));
#4044=EDGE_LOOP('',(#9447));
#4045=EDGE_LOOP('',(#9448));
#4046=EDGE_LOOP('',(#9449));
#4047=EDGE_LOOP('',(#9450));
#4048=EDGE_LOOP('',(#9451));
#4049=EDGE_LOOP('',(#9452));
#4050=EDGE_LOOP('',(#9453));
#4051=EDGE_LOOP('',(#9454));
#4052=EDGE_LOOP('',(#9455));
#4053=EDGE_LOOP('',(#9456));
#4054=EDGE_LOOP('',(#9457));
#4055=EDGE_LOOP('',(#9458));
#4056=EDGE_LOOP('',(#9459));
#4057=EDGE_LOOP('',(#9460));
#4058=EDGE_LOOP('',(#9461));
#4059=EDGE_LOOP('',(#9462));
#4060=EDGE_LOOP('',(#9463));
#4061=EDGE_LOOP('',(#9464));
#4062=EDGE_LOOP('',(#9465));
#4063=EDGE_LOOP('',(#9466,#9467,#9468,#9469));
#4064=EDGE_LOOP('',(#9470,#9471,#9472,#9473));
#4065=EDGE_LOOP('',(#9474,#9475,#9476,#9477));
#4066=EDGE_LOOP('',(#9478,#9479,#9480,#9481));
#4067=EDGE_LOOP('',(#9482,#9483,#9484,#9485));
#4068=EDGE_LOOP('',(#9486,#9487,#9488,#9489));
#4069=EDGE_LOOP('',(#9490,#9491,#9492,#9493));
#4070=EDGE_LOOP('',(#9494,#9495,#9496,#9497));
#4071=EDGE_LOOP('',(#9498,#9499,#9500,#9501));
#4072=EDGE_LOOP('',(#9502,#9503,#9504,#9505));
#4073=EDGE_LOOP('',(#9506,#9507,#9508,#9509));
#4074=EDGE_LOOP('',(#9510,#9511,#9512,#9513));
#4075=EDGE_LOOP('',(#9514,#9515,#9516,#9517));
#4076=EDGE_LOOP('',(#9518,#9519,#9520,#9521));
#4077=EDGE_LOOP('',(#9522,#9523,#9524,#9525));
#4078=EDGE_LOOP('',(#9526,#9527,#9528,#9529));
#4079=EDGE_LOOP('',(#9530,#9531,#9532,#9533));
#4080=EDGE_LOOP('',(#9534,#9535,#9536,#9537));
#4081=EDGE_LOOP('',(#9538,#9539,#9540,#9541));
#4082=EDGE_LOOP('',(#9542,#9543,#9544,#9545));
#4083=EDGE_LOOP('',(#9546,#9547,#9548,#9549));
#4084=EDGE_LOOP('',(#9550,#9551,#9552,#9553));
#4085=EDGE_LOOP('',(#9554,#9555,#9556,#9557));
#4086=EDGE_LOOP('',(#9558,#9559,#9560,#9561));
#4087=EDGE_LOOP('',(#9562,#9563,#9564,#9565));
#4088=EDGE_LOOP('',(#9566,#9567,#9568,#9569));
#4089=EDGE_LOOP('',(#9570,#9571,#9572,#9573));
#4090=EDGE_LOOP('',(#9574,#9575,#9576,#9577));
#4091=EDGE_LOOP('',(#9578,#9579,#9580,#9581));
#4092=EDGE_LOOP('',(#9582,#9583,#9584,#9585));
#4093=EDGE_LOOP('',(#9586,#9587,#9588,#9589));
#4094=EDGE_LOOP('',(#9590,#9591,#9592,#9593));
#4095=EDGE_LOOP('',(#9594,#9595,#9596,#9597));
#4096=EDGE_LOOP('',(#9598,#9599,#9600,#9601));
#4097=EDGE_LOOP('',(#9602,#9603,#9604,#9605));
#4098=EDGE_LOOP('',(#9606,#9607,#9608,#9609));
#4099=EDGE_LOOP('',(#9610,#9611,#9612,#9613));
#4100=EDGE_LOOP('',(#9614,#9615,#9616,#9617));
#4101=EDGE_LOOP('',(#9618,#9619,#9620,#9621));
#4102=EDGE_LOOP('',(#9622,#9623,#9624,#9625));
#4103=EDGE_LOOP('',(#9626,#9627,#9628,#9629));
#4104=EDGE_LOOP('',(#9630,#9631,#9632,#9633));
#4105=EDGE_LOOP('',(#9634,#9635,#9636,#9637));
#4106=EDGE_LOOP('',(#9638,#9639,#9640,#9641));
#4107=EDGE_LOOP('',(#9642,#9643,#9644,#9645));
#4108=EDGE_LOOP('',(#9646,#9647,#9648,#9649));
#4109=EDGE_LOOP('',(#9650,#9651,#9652,#9653));
#4110=EDGE_LOOP('',(#9654,#9655,#9656,#9657));
#4111=EDGE_LOOP('',(#9658,#9659,#9660,#9661,#9662,#9663,#9664,#9665,#9666,
#9667,#9668,#9669));
#4112=EDGE_LOOP('',(#9670,#9671,#9672,#9673));
#4113=EDGE_LOOP('',(#9674));
#4114=EDGE_LOOP('',(#9675));
#4115=EDGE_LOOP('',(#9676));
#4116=EDGE_LOOP('',(#9677));
#4117=EDGE_LOOP('',(#9678));
#4118=EDGE_LOOP('',(#9679));
#4119=EDGE_LOOP('',(#9680));
#4120=EDGE_LOOP('',(#9681));
#4121=EDGE_LOOP('',(#9682));
#4122=EDGE_LOOP('',(#9683));
#4123=EDGE_LOOP('',(#9684));
#4124=EDGE_LOOP('',(#9685));
#4125=EDGE_LOOP('',(#9686));
#4126=EDGE_LOOP('',(#9687));
#4127=EDGE_LOOP('',(#9688));
#4128=EDGE_LOOP('',(#9689));
#4129=EDGE_LOOP('',(#9690));
#4130=EDGE_LOOP('',(#9691));
#4131=EDGE_LOOP('',(#9692));
#4132=EDGE_LOOP('',(#9693));
#4133=EDGE_LOOP('',(#9694));
#4134=EDGE_LOOP('',(#9695));
#4135=EDGE_LOOP('',(#9696));
#4136=EDGE_LOOP('',(#9697));
#4137=EDGE_LOOP('',(#9698));
#4138=EDGE_LOOP('',(#9699));
#4139=EDGE_LOOP('',(#9700));
#4140=EDGE_LOOP('',(#9701));
#4141=EDGE_LOOP('',(#9702));
#4142=EDGE_LOOP('',(#9703));
#4143=EDGE_LOOP('',(#9704));
#4144=EDGE_LOOP('',(#9705));
#4145=EDGE_LOOP('',(#9706));
#4146=EDGE_LOOP('',(#9707));
#4147=EDGE_LOOP('',(#9708));
#4148=EDGE_LOOP('',(#9709));
#4149=EDGE_LOOP('',(#9710));
#4150=EDGE_LOOP('',(#9711));
#4151=EDGE_LOOP('',(#9712));
#4152=EDGE_LOOP('',(#9713));
#4153=EDGE_LOOP('',(#9714));
#4154=EDGE_LOOP('',(#9715));
#4155=EDGE_LOOP('',(#9716));
#4156=EDGE_LOOP('',(#9717));
#4157=EDGE_LOOP('',(#9718));
#4158=EDGE_LOOP('',(#9719));
#4159=EDGE_LOOP('',(#9720));
#4160=EDGE_LOOP('',(#9721,#9722,#9723,#9724));
#4161=EDGE_LOOP('',(#9725));
#4162=EDGE_LOOP('',(#9726));
#4163=EDGE_LOOP('',(#9727));
#4164=EDGE_LOOP('',(#9728));
#4165=EDGE_LOOP('',(#9729));
#4166=EDGE_LOOP('',(#9730));
#4167=EDGE_LOOP('',(#9731));
#4168=EDGE_LOOP('',(#9732));
#4169=EDGE_LOOP('',(#9733));
#4170=EDGE_LOOP('',(#9734));
#4171=EDGE_LOOP('',(#9735));
#4172=EDGE_LOOP('',(#9736));
#4173=EDGE_LOOP('',(#9737));
#4174=EDGE_LOOP('',(#9738));
#4175=EDGE_LOOP('',(#9739));
#4176=EDGE_LOOP('',(#9740));
#4177=EDGE_LOOP('',(#9741));
#4178=EDGE_LOOP('',(#9742));
#4179=EDGE_LOOP('',(#9743));
#4180=EDGE_LOOP('',(#9744));
#4181=EDGE_LOOP('',(#9745));
#4182=EDGE_LOOP('',(#9746));
#4183=EDGE_LOOP('',(#9747));
#4184=EDGE_LOOP('',(#9748));
#4185=EDGE_LOOP('',(#9749));
#4186=EDGE_LOOP('',(#9750));
#4187=EDGE_LOOP('',(#9751));
#4188=EDGE_LOOP('',(#9752));
#4189=EDGE_LOOP('',(#9753));
#4190=EDGE_LOOP('',(#9754));
#4191=EDGE_LOOP('',(#9755));
#4192=EDGE_LOOP('',(#9756));
#4193=EDGE_LOOP('',(#9757));
#4194=EDGE_LOOP('',(#9758));
#4195=EDGE_LOOP('',(#9759));
#4196=EDGE_LOOP('',(#9760));
#4197=EDGE_LOOP('',(#9761));
#4198=EDGE_LOOP('',(#9762));
#4199=EDGE_LOOP('',(#9763));
#4200=EDGE_LOOP('',(#9764));
#4201=EDGE_LOOP('',(#9765));
#4202=EDGE_LOOP('',(#9766));
#4203=EDGE_LOOP('',(#9767));
#4204=EDGE_LOOP('',(#9768));
#4205=EDGE_LOOP('',(#9769));
#4206=EDGE_LOOP('',(#9770));
#4207=EDGE_LOOP('',(#9771));
#4208=EDGE_LOOP('',(#9772,#9773,#9774,#9775));
#4209=EDGE_LOOP('',(#9776,#9777,#9778,#9779));
#4210=EDGE_LOOP('',(#9780,#9781,#9782,#9783));
#4211=EDGE_LOOP('',(#9784,#9785,#9786,#9787));
#4212=EDGE_LOOP('',(#9788,#9789,#9790,#9791,#9792,#9793,#9794,#9795));
#4213=EDGE_LOOP('',(#9796));
#4214=EDGE_LOOP('',(#9797));
#4215=EDGE_LOOP('',(#9798));
#4216=EDGE_LOOP('',(#9799));
#4217=EDGE_LOOP('',(#9800));
#4218=EDGE_LOOP('',(#9801));
#4219=EDGE_LOOP('',(#9802));
#4220=EDGE_LOOP('',(#9803));
#4221=EDGE_LOOP('',(#9804));
#4222=EDGE_LOOP('',(#9805));
#4223=EDGE_LOOP('',(#9806));
#4224=EDGE_LOOP('',(#9807,#9808,#9809,#9810));
#4225=EDGE_LOOP('',(#9811,#9812,#9813,#9814,#9815,#9816,#9817,#9818));
#4226=EDGE_LOOP('',(#9819));
#4227=EDGE_LOOP('',(#9820));
#4228=EDGE_LOOP('',(#9821));
#4229=EDGE_LOOP('',(#9822));
#4230=EDGE_LOOP('',(#9823));
#4231=EDGE_LOOP('',(#9824));
#4232=EDGE_LOOP('',(#9825));
#4233=EDGE_LOOP('',(#9826));
#4234=EDGE_LOOP('',(#9827));
#4235=EDGE_LOOP('',(#9828));
#4236=EDGE_LOOP('',(#9829));
#4237=EDGE_LOOP('',(#9830,#9831,#9832,#9833));
#4238=EDGE_LOOP('',(#9834,#9835,#9836,#9837));
#4239=EDGE_LOOP('',(#9838,#9839,#9840,#9841));
#4240=EDGE_LOOP('',(#9842,#9843,#9844,#9845));
#4241=EDGE_LOOP('',(#9846,#9847,#9848,#9849));
#4242=EDGE_LOOP('',(#9850,#9851,#9852,#9853));
#4243=EDGE_LOOP('',(#9854,#9855,#9856,#9857));
#4244=EDGE_LOOP('',(#9858,#9859,#9860,#9861));
#4245=EDGE_LOOP('',(#9862,#9863,#9864,#9865));
#4246=EDGE_LOOP('',(#9866,#9867,#9868,#9869));
#4247=EDGE_LOOP('',(#9870,#9871,#9872,#9873));
#4248=EDGE_LOOP('',(#9874,#9875,#9876,#9877));
#4249=EDGE_LOOP('',(#9878,#9879,#9880,#9881));
#4250=EDGE_LOOP('',(#9882,#9883,#9884,#9885));
#4251=EDGE_LOOP('',(#9886,#9887,#9888,#9889));
#4252=EDGE_LOOP('',(#9890,#9891,#9892,#9893));
#4253=EDGE_LOOP('',(#9894,#9895,#9896,#9897,#9898,#9899,#9900,#9901));
#4254=EDGE_LOOP('',(#9902));
#4255=EDGE_LOOP('',(#9903));
#4256=EDGE_LOOP('',(#9904));
#4257=EDGE_LOOP('',(#9905));
#4258=EDGE_LOOP('',(#9906));
#4259=EDGE_LOOP('',(#9907));
#4260=EDGE_LOOP('',(#9908));
#4261=EDGE_LOOP('',(#9909));
#4262=EDGE_LOOP('',(#9910));
#4263=EDGE_LOOP('',(#9911));
#4264=EDGE_LOOP('',(#9912));
#4265=EDGE_LOOP('',(#9913,#9914,#9915,#9916));
#4266=EDGE_LOOP('',(#9917,#9918,#9919,#9920));
#4267=EDGE_LOOP('',(#9921,#9922,#9923,#9924));
#4268=EDGE_LOOP('',(#9925,#9926,#9927,#9928));
#4269=EDGE_LOOP('',(#9929,#9930,#9931,#9932));
#4270=EDGE_LOOP('',(#9933,#9934,#9935,#9936));
#4271=EDGE_LOOP('',(#9937,#9938,#9939,#9940));
#4272=EDGE_LOOP('',(#9941,#9942,#9943,#9944));
#4273=EDGE_LOOP('',(#9945,#9946,#9947,#9948));
#4274=EDGE_LOOP('',(#9949,#9950,#9951,#9952));
#4275=EDGE_LOOP('',(#9953,#9954,#9955,#9956));
#4276=EDGE_LOOP('',(#9957,#9958,#9959,#9960));
#4277=EDGE_LOOP('',(#9961,#9962,#9963,#9964));
#4278=EDGE_LOOP('',(#9965,#9966,#9967,#9968));
#4279=EDGE_LOOP('',(#9969,#9970,#9971,#9972));
#4280=EDGE_LOOP('',(#9973,#9974,#9975,#9976));
#4281=EDGE_LOOP('',(#9977,#9978,#9979,#9980,#9981,#9982,#9983,#9984));
#4282=EDGE_LOOP('',(#9985));
#4283=EDGE_LOOP('',(#9986));
#4284=EDGE_LOOP('',(#9987));
#4285=EDGE_LOOP('',(#9988));
#4286=EDGE_LOOP('',(#9989));
#4287=EDGE_LOOP('',(#9990));
#4288=EDGE_LOOP('',(#9991));
#4289=EDGE_LOOP('',(#9992));
#4290=EDGE_LOOP('',(#9993));
#4291=EDGE_LOOP('',(#9994));
#4292=EDGE_LOOP('',(#9995));
#4293=EDGE_LOOP('',(#9996,#9997,#9998,#9999));
#4294=EDGE_LOOP('',(#10000));
#4295=EDGE_LOOP('',(#10001));
#4296=EDGE_LOOP('',(#10002));
#4297=EDGE_LOOP('',(#10003,#10004,#10005,#10006));
#4298=EDGE_LOOP('',(#10007));
#4299=EDGE_LOOP('',(#10008,#10009,#10010,#10011,#10012,#10013,#10014,#10015,
#10016,#10017,#10018,#10019));
#4300=EDGE_LOOP('',(#10020,#10021,#10022,#10023));
#4301=EDGE_LOOP('',(#10024));
#4302=EDGE_LOOP('',(#10025));
#4303=EDGE_LOOP('',(#10026,#10027,#10028,#10029,#10030,#10031,#10032,#10033,
#10034,#10035,#10036,#10037));
#4304=EDGE_LOOP('',(#10038,#10039,#10040,#10041));
#4305=EDGE_LOOP('',(#10042,#10043,#10044,#10045));
#4306=EDGE_LOOP('',(#10046,#10047,#10048,#10049));
#4307=EDGE_LOOP('',(#10050,#10051,#10052,#10053));
#4308=EDGE_LOOP('',(#10054,#10055,#10056,#10057));
#4309=EDGE_LOOP('',(#10058,#10059,#10060,#10061));
#4310=EDGE_LOOP('',(#10062,#10063,#10064,#10065));
#4311=EDGE_LOOP('',(#10066,#10067,#10068,#10069));
#4312=EDGE_LOOP('',(#10070,#10071,#10072,#10073,#10074,#10075));
#4313=EDGE_LOOP('',(#10076));
#4314=EDGE_LOOP('',(#10077,#10078,#10079,#10080,#10081,#10082));
#4315=EDGE_LOOP('',(#10083));
#4316=EDGE_LOOP('',(#10084,#10085,#10086,#10087));
#4317=EDGE_LOOP('',(#10088,#10089,#10090,#10091));
#4318=EDGE_LOOP('',(#10092,#10093,#10094,#10095));
#4319=EDGE_LOOP('',(#10096,#10097,#10098,#10099));
#4320=EDGE_LOOP('',(#10100,#10101,#10102,#10103,#10104,#10105,#10106,#10107));
#4321=EDGE_LOOP('',(#10108));
#4322=EDGE_LOOP('',(#10109));
#4323=EDGE_LOOP('',(#10110));
#4324=EDGE_LOOP('',(#10111));
#4325=EDGE_LOOP('',(#10112));
#4326=EDGE_LOOP('',(#10113));
#4327=EDGE_LOOP('',(#10114));
#4328=EDGE_LOOP('',(#10115));
#4329=EDGE_LOOP('',(#10116));
#4330=EDGE_LOOP('',(#10117));
#4331=EDGE_LOOP('',(#10118));
#4332=EDGE_LOOP('',(#10119,#10120,#10121,#10122));
#4333=EDGE_LOOP('',(#10123,#10124,#10125,#10126,#10127,#10128,#10129,#10130));
#4334=EDGE_LOOP('',(#10131));
#4335=EDGE_LOOP('',(#10132));
#4336=EDGE_LOOP('',(#10133));
#4337=EDGE_LOOP('',(#10134));
#4338=EDGE_LOOP('',(#10135));
#4339=EDGE_LOOP('',(#10136));
#4340=EDGE_LOOP('',(#10137));
#4341=EDGE_LOOP('',(#10138));
#4342=EDGE_LOOP('',(#10139));
#4343=EDGE_LOOP('',(#10140));
#4344=EDGE_LOOP('',(#10141));
#4345=EDGE_LOOP('',(#10142,#10143,#10144,#10145));
#4346=EDGE_LOOP('',(#10146,#10147,#10148,#10149));
#4347=EDGE_LOOP('',(#10150,#10151,#10152,#10153));
#4348=EDGE_LOOP('',(#10154,#10155,#10156,#10157));
#4349=EDGE_LOOP('',(#10158,#10159,#10160,#10161));
#4350=EDGE_LOOP('',(#10162,#10163,#10164,#10165));
#4351=EDGE_LOOP('',(#10166,#10167,#10168,#10169));
#4352=EDGE_LOOP('',(#10170,#10171,#10172,#10173));
#4353=EDGE_LOOP('',(#10174,#10175,#10176,#10177));
#4354=EDGE_LOOP('',(#10178,#10179,#10180,#10181));
#4355=EDGE_LOOP('',(#10182,#10183,#10184,#10185));
#4356=EDGE_LOOP('',(#10186,#10187,#10188,#10189));
#4357=EDGE_LOOP('',(#10190,#10191,#10192,#10193));
#4358=EDGE_LOOP('',(#10194,#10195,#10196,#10197));
#4359=EDGE_LOOP('',(#10198,#10199,#10200,#10201));
#4360=EDGE_LOOP('',(#10202,#10203,#10204,#10205));
#4361=EDGE_LOOP('',(#10206,#10207,#10208,#10209,#10210,#10211,#10212,#10213));
#4362=EDGE_LOOP('',(#10214));
#4363=EDGE_LOOP('',(#10215));
#4364=EDGE_LOOP('',(#10216));
#4365=EDGE_LOOP('',(#10217));
#4366=EDGE_LOOP('',(#10218));
#4367=EDGE_LOOP('',(#10219));
#4368=EDGE_LOOP('',(#10220));
#4369=EDGE_LOOP('',(#10221));
#4370=EDGE_LOOP('',(#10222));
#4371=EDGE_LOOP('',(#10223));
#4372=EDGE_LOOP('',(#10224));
#4373=EDGE_LOOP('',(#10225,#10226,#10227,#10228));
#4374=EDGE_LOOP('',(#10229,#10230,#10231,#10232));
#4375=EDGE_LOOP('',(#10233,#10234,#10235,#10236));
#4376=EDGE_LOOP('',(#10237,#10238,#10239,#10240));
#4377=EDGE_LOOP('',(#10241,#10242,#10243,#10244));
#4378=EDGE_LOOP('',(#10245,#10246,#10247,#10248));
#4379=EDGE_LOOP('',(#10249,#10250,#10251,#10252));
#4380=EDGE_LOOP('',(#10253,#10254,#10255,#10256));
#4381=EDGE_LOOP('',(#10257,#10258,#10259,#10260));
#4382=EDGE_LOOP('',(#10261,#10262,#10263,#10264));
#4383=EDGE_LOOP('',(#10265,#10266,#10267,#10268));
#4384=EDGE_LOOP('',(#10269,#10270,#10271,#10272));
#4385=EDGE_LOOP('',(#10273,#10274,#10275,#10276));
#4386=EDGE_LOOP('',(#10277,#10278,#10279,#10280));
#4387=EDGE_LOOP('',(#10281,#10282,#10283,#10284));
#4388=EDGE_LOOP('',(#10285,#10286,#10287,#10288));
#4389=EDGE_LOOP('',(#10289,#10290,#10291,#10292,#10293,#10294,#10295,#10296));
#4390=EDGE_LOOP('',(#10297));
#4391=EDGE_LOOP('',(#10298));
#4392=EDGE_LOOP('',(#10299));
#4393=EDGE_LOOP('',(#10300));
#4394=EDGE_LOOP('',(#10301));
#4395=EDGE_LOOP('',(#10302));
#4396=EDGE_LOOP('',(#10303));
#4397=EDGE_LOOP('',(#10304));
#4398=EDGE_LOOP('',(#10305));
#4399=EDGE_LOOP('',(#10306));
#4400=EDGE_LOOP('',(#10307));
#4401=EDGE_LOOP('',(#10308,#10309,#10310,#10311));
#4402=EDGE_LOOP('',(#10312));
#4403=EDGE_LOOP('',(#10313));
#4404=EDGE_LOOP('',(#10314));
#4405=EDGE_LOOP('',(#10315,#10316,#10317,#10318));
#4406=EDGE_LOOP('',(#10319));
#4407=EDGE_LOOP('',(#10320,#10321,#10322,#10323,#10324,#10325,#10326,#10327,
#10328,#10329,#10330,#10331));
#4408=EDGE_LOOP('',(#10332,#10333,#10334,#10335));
#4409=EDGE_LOOP('',(#10336));
#4410=EDGE_LOOP('',(#10337));
#4411=EDGE_LOOP('',(#10338,#10339,#10340,#10341,#10342,#10343,#10344,#10345,
#10346,#10347,#10348,#10349));
#4412=EDGE_LOOP('',(#10350,#10351,#10352,#10353));
#4413=EDGE_LOOP('',(#10354,#10355,#10356,#10357,#10358,#10359));
#4414=EDGE_LOOP('',(#10360));
#4415=EDGE_LOOP('',(#10361,#10362,#10363,#10364));
#4416=EDGE_LOOP('',(#10365,#10366,#10367,#10368));
#4417=EDGE_LOOP('',(#10369,#10370,#10371,#10372));
#4418=EDGE_LOOP('',(#10373,#10374,#10375,#10376));
#4419=EDGE_LOOP('',(#10377,#10378,#10379,#10380));
#4420=EDGE_LOOP('',(#10381,#10382,#10383,#10384));
#4421=EDGE_LOOP('',(#10385,#10386,#10387,#10388,#10389,#10390));
#4422=EDGE_LOOP('',(#10391,#10392,#10393,#10394));
#4423=EDGE_LOOP('',(#10395));
#4424=EDGE_LOOP('',(#10396,#10397,#10398,#10399));
#4425=EDGE_LOOP('',(#10400,#10401,#10402,#10403));
#4426=EDGE_LOOP('',(#10404,#10405,#10406,#10407));
#4427=EDGE_LOOP('',(#10408,#10409,#10410,#10411));
#4428=EDGE_LOOP('',(#10412,#10413,#10414,#10415));
#4429=EDGE_LOOP('',(#10416,#10417,#10418,#10419));
#4430=EDGE_LOOP('',(#10420,#10421,#10422,#10423));
#4431=EDGE_LOOP('',(#10424,#10425,#10426,#10427,#10428,#10429));
#4432=EDGE_LOOP('',(#10430));
#4433=EDGE_LOOP('',(#10431,#10432,#10433,#10434,#10435,#10436));
#4434=EDGE_LOOP('',(#10437));
#4435=EDGE_LOOP('',(#10438,#10439,#10440,#10441));
#4436=EDGE_LOOP('',(#10442,#10443,#10444,#10445));
#4437=EDGE_LOOP('',(#10446,#10447,#10448,#10449));
#4438=EDGE_LOOP('',(#10450,#10451,#10452,#10453));
#4439=EDGE_LOOP('',(#10454,#10455,#10456,#10457));
#4440=EDGE_LOOP('',(#10458,#10459,#10460,#10461));
#4441=EDGE_LOOP('',(#10462,#10463,#10464,#10465));
#4442=EDGE_LOOP('',(#10466,#10467,#10468,#10469,#10470,#10471));
#4443=EDGE_LOOP('',(#10472));
#4444=EDGE_LOOP('',(#10473,#10474,#10475,#10476,#10477,#10478));
#4445=EDGE_LOOP('',(#10479));
#4446=EDGE_LOOP('',(#10480,#10481,#10482,#10483));
#4447=EDGE_LOOP('',(#10484,#10485,#10486,#10487));
#4448=EDGE_LOOP('',(#10488,#10489,#10490,#10491));
#4449=EDGE_LOOP('',(#10492,#10493,#10494,#10495));
#4450=EDGE_LOOP('',(#10496,#10497,#10498,#10499));
#4451=EDGE_LOOP('',(#10500,#10501,#10502,#10503));
#4452=EDGE_LOOP('',(#10504,#10505,#10506,#10507));
#4453=EDGE_LOOP('',(#10508,#10509,#10510,#10511));
#4454=EDGE_LOOP('',(#10512,#10513,#10514,#10515));
#4455=EDGE_LOOP('',(#10516,#10517,#10518,#10519));
#4456=EDGE_LOOP('',(#10520,#10521,#10522,#10523));
#4457=EDGE_LOOP('',(#10524,#10525,#10526,#10527));
#4458=EDGE_LOOP('',(#10528,#10529,#10530,#10531));
#4459=EDGE_LOOP('',(#10532,#10533,#10534,#10535));
#4460=EDGE_LOOP('',(#10536,#10537,#10538,#10539));
#4461=EDGE_LOOP('',(#10540,#10541,#10542,#10543));
#4462=EDGE_LOOP('',(#10544,#10545,#10546,#10547));
#4463=EDGE_LOOP('',(#10548,#10549,#10550,#10551));
#4464=EDGE_LOOP('',(#10552,#10553,#10554,#10555));
#4465=EDGE_LOOP('',(#10556,#10557,#10558,#10559));
#4466=EDGE_LOOP('',(#10560,#10561,#10562,#10563));
#4467=EDGE_LOOP('',(#10564,#10565,#10566,#10567));
#4468=EDGE_LOOP('',(#10568,#10569,#10570,#10571));
#4469=EDGE_LOOP('',(#10572,#10573,#10574,#10575));
#4470=EDGE_LOOP('',(#10576,#10577,#10578,#10579));
#4471=EDGE_LOOP('',(#10580,#10581,#10582,#10583));
#4472=EDGE_LOOP('',(#10584,#10585,#10586,#10587));
#4473=EDGE_LOOP('',(#10588,#10589,#10590,#10591));
#4474=EDGE_LOOP('',(#10592,#10593,#10594,#10595));
#4475=EDGE_LOOP('',(#10596,#10597,#10598,#10599));
#4476=EDGE_LOOP('',(#10600,#10601,#10602,#10603));
#4477=EDGE_LOOP('',(#10604,#10605,#10606,#10607));
#4478=EDGE_LOOP('',(#10608,#10609,#10610,#10611));
#4479=EDGE_LOOP('',(#10612,#10613,#10614,#10615));
#4480=EDGE_LOOP('',(#10616,#10617,#10618,#10619));
#4481=EDGE_LOOP('',(#10620,#10621,#10622,#10623));
#4482=EDGE_LOOP('',(#10624,#10625,#10626,#10627));
#4483=EDGE_LOOP('',(#10628,#10629,#10630,#10631));
#4484=EDGE_LOOP('',(#10632,#10633,#10634,#10635));
#4485=EDGE_LOOP('',(#10636,#10637,#10638,#10639));
#4486=EDGE_LOOP('',(#10640,#10641,#10642,#10643,#10644,#10645,#10646,#10647,
#10648,#10649,#10650,#10651,#10652,#10653,#10654,#10655,#10656,#10657,#10658,
#10659,#10660,#10661,#10662,#10663,#10664,#10665,#10666,#10667,#10668,#10669));
#4487=EDGE_LOOP('',(#10670,#10671,#10672,#10673,#10674,#10675,#10676,#10677,
#10678,#10679));
#4488=EDGE_LOOP('',(#10680,#10681,#10682,#10683,#10684,#10685,#10686,#10687,
#10688,#10689,#10690,#10691,#10692,#10693,#10694,#10695,#10696,#10697,#10698,
#10699,#10700,#10701,#10702,#10703,#10704,#10705,#10706,#10707,#10708,#10709));
#4489=EDGE_LOOP('',(#10710,#10711,#10712,#10713,#10714,#10715,#10716,#10717,
#10718,#10719));
#4490=EDGE_LOOP('',(#10720,#10721,#10722,#10723));
#4491=EDGE_LOOP('',(#10724,#10725,#10726,#10727));
#4492=EDGE_LOOP('',(#10728,#10729,#10730,#10731));
#4493=EDGE_LOOP('',(#10732,#10733,#10734,#10735));
#4494=EDGE_LOOP('',(#10736,#10737,#10738,#10739));
#4495=EDGE_LOOP('',(#10740,#10741,#10742,#10743));
#4496=EDGE_LOOP('',(#10744,#10745,#10746,#10747));
#4497=EDGE_LOOP('',(#10748,#10749,#10750,#10751,#10752,#10753));
#4498=EDGE_LOOP('',(#10754));
#4499=EDGE_LOOP('',(#10755,#10756,#10757,#10758,#10759,#10760));
#4500=EDGE_LOOP('',(#10761));
#4501=CIRCLE('',#11486,20.7480593298244);
#4502=CIRCLE('',#11487,0.5);
#4503=CIRCLE('',#11488,21.2480593298244);
#4504=CIRCLE('',#11489,21.2480593298244);
#4505=CIRCLE('',#11491,21.2480593298244);
#4506=CIRCLE('',#11492,21.2480593298244);
#4507=CIRCLE('',#11495,0.5);
#4508=CIRCLE('',#11496,20.7480593298244);
#4509=CIRCLE('',#11498,21.2480593298244);
#4510=CIRCLE('',#11499,0.5);
#4511=CIRCLE('',#11500,20.7480593298244);
#4512=CIRCLE('',#11501,21.2480593298244);
#4513=CIRCLE('',#11503,21.2480593298244);
#4514=CIRCLE('',#11504,21.2480593298244);
#4515=CIRCLE('',#11506,0.5);
#4516=CIRCLE('',#11508,6.);
#4517=CIRCLE('',#11510,6.);
#4518=CIRCLE('',#11512,20.7480593298244);
#4519=CIRCLE('',#11513,0.5);
#4520=CIRCLE('',#11514,21.2480593298244);
#4521=CIRCLE('',#11515,21.2480593298244);
#4522=CIRCLE('',#11517,21.2480593298244);
#4523=CIRCLE('',#11518,21.2480593298244);
#4524=CIRCLE('',#11521,0.5);
#4525=CIRCLE('',#11524,20.7480593298244);
#4526=CIRCLE('',#11525,16.7480593298244);
#4527=CIRCLE('',#11527,20.7480593298244);
#4528=CIRCLE('',#11529,15.7480593298244);
#4529=CIRCLE('',#11531,20.7480593298244);
#4530=CIRCLE('',#11532,16.7480593298244);
#4531=CIRCLE('',#11534,20.7480593298244);
#4532=CIRCLE('',#11535,16.7480593298244);
#4533=CIRCLE('',#11539,20.7480593298244);
#4534=CIRCLE('',#11540,16.7480593298244);
#4535=CIRCLE('',#11542,20.7480593298244);
#4536=CIRCLE('',#11544,15.7480593298244);
#4537=CIRCLE('',#11546,15.7480593298244);
#4538=CIRCLE('',#11548,15.7480593298244);
#4539=CIRCLE('',#11551,6.);
#4540=CIRCLE('',#11553,6.);
#4541=CIRCLE('',#11557,1.);
#4542=CIRCLE('',#11558,1.);
#4543=CIRCLE('',#11560,2.5);
#4544=CIRCLE('',#11561,2.5);
#4545=CIRCLE('',#11562,2.5);
#4546=CIRCLE('',#11563,7.5);
#4547=CIRCLE('',#11564,2.5);
#4548=CIRCLE('',#11565,2.5);
#4549=CIRCLE('',#11566,2.5);
#4550=CIRCLE('',#11567,2.5);
#4551=CIRCLE('',#11568,2.5);
#4552=CIRCLE('',#11569,2.5);
#4553=CIRCLE('',#11570,2.5);
#4554=CIRCLE('',#11572,1.);
#4555=CIRCLE('',#11574,1.);
#4556=CIRCLE('',#11576,2.5);
#4557=CIRCLE('',#11577,2.5);
#4558=CIRCLE('',#11579,2.5);
#4559=CIRCLE('',#11580,2.5);
#4560=CIRCLE('',#11582,2.5);
#4561=CIRCLE('',#11583,2.5);
#4562=CIRCLE('',#11585,7.5);
#4563=CIRCLE('',#11586,7.5);
#4564=CIRCLE('',#11588,2.5);
#4565=CIRCLE('',#11589,2.5);
#4566=CIRCLE('',#11591,2.5);
#4567=CIRCLE('',#11592,2.5);
#4568=CIRCLE('',#11594,2.5);
#4569=CIRCLE('',#11595,2.5);
#4570=CIRCLE('',#11597,2.5);
#4571=CIRCLE('',#11598,2.5);
#4572=CIRCLE('',#11600,2.5);
#4573=CIRCLE('',#11601,2.5);
#4574=CIRCLE('',#11603,2.5);
#4575=CIRCLE('',#11604,2.5);
#4576=CIRCLE('',#11606,2.5);
#4577=CIRCLE('',#11607,2.5);
#4578=CIRCLE('',#11609,2.5);
#4579=CIRCLE('',#11611,2.5);
#4580=CIRCLE('',#11613,2.5);
#4581=CIRCLE('',#11615,2.5);
#4582=CIRCLE('',#11617,2.5);
#4583=CIRCLE('',#11619,2.5);
#4584=CIRCLE('',#11621,2.5);
#4585=CIRCLE('',#11623,7.5);
#4586=CIRCLE('',#11625,2.5);
#4587=CIRCLE('',#11627,2.5);
#4588=CIRCLE('',#11629,2.5);
#4589=CIRCLE('',#11631,2.5);
#4590=CIRCLE('',#11632,2.5);
#4591=CIRCLE('',#11634,2.5);
#4592=CIRCLE('',#11635,2.5);
#4593=CIRCLE('',#11637,2.5);
#4594=CIRCLE('',#11638,2.5);
#4595=CIRCLE('',#11640,7.5);
#4596=CIRCLE('',#11641,7.5);
#4597=CIRCLE('',#11643,2.5);
#4598=CIRCLE('',#11644,2.5);
#4599=CIRCLE('',#11646,2.5);
#4600=CIRCLE('',#11647,2.5);
#4601=CIRCLE('',#11649,2.5);
#4602=CIRCLE('',#11650,2.5);
#4603=CIRCLE('',#11652,2.5);
#4604=CIRCLE('',#11653,2.5);
#4605=CIRCLE('',#11655,2.5);
#4606=CIRCLE('',#11656,2.5);
#4607=CIRCLE('',#11658,2.5);
#4608=CIRCLE('',#11659,2.5);
#4609=CIRCLE('',#11661,2.5);
#4610=CIRCLE('',#11662,2.5);
#4611=CIRCLE('',#11673,1.4635);
#4612=CIRCLE('',#11682,1.4635);
#4613=CIRCLE('',#11687,0.999999999999975);
#4614=CIRCLE('',#11688,0.999999999999975);
#4615=CIRCLE('',#11692,1.99999999999998);
#4616=CIRCLE('',#11693,1.99999999999998);
#4617=CIRCLE('',#11696,0.500000000000007);
#4618=CIRCLE('',#11697,0.500000000000007);
#4619=CIRCLE('',#11699,0.499999999999998);
#4620=CIRCLE('',#11700,0.499999999999998);
#4621=CIRCLE('',#11704,0.999999999999975);
#4622=CIRCLE('',#11705,0.999999999999975);
#4623=CIRCLE('',#11709,1.99999999999998);
#4624=CIRCLE('',#11710,1.99999999999998);
#4625=CIRCLE('',#11713,0.500000000000007);
#4626=CIRCLE('',#11714,0.500000000000007);
#4627=CIRCLE('',#11717,0.499999999999998);
#4628=CIRCLE('',#11718,0.499999999999998);
#4629=CIRCLE('',#11723,0.999999999999981);
#4630=CIRCLE('',#11724,0.999999999999981);
#4631=CIRCLE('',#11727,0.999999999999967);
#4632=CIRCLE('',#11728,0.999999999999967);
#4633=CIRCLE('',#11733,1.99999999999997);
#4634=CIRCLE('',#11734,1.99999999999997);
#4635=CIRCLE('',#11737,1.99999999999998);
#4636=CIRCLE('',#11738,1.99999999999998);
#4637=CIRCLE('',#11741,0.999999999999981);
#4638=CIRCLE('',#11742,0.999999999999981);
#4639=CIRCLE('',#11745,0.999999999999967);
#4640=CIRCLE('',#11746,0.999999999999967);
#4641=CIRCLE('',#11751,1.99999999999997);
#4642=CIRCLE('',#11752,1.99999999999997);
#4643=CIRCLE('',#11755,1.99999999999998);
#4644=CIRCLE('',#11756,1.99999999999998);
#4645=CIRCLE('',#11761,2.5);
#4646=CIRCLE('',#11762,2.5);
#4647=CIRCLE('',#11764,2.5);
#4648=CIRCLE('',#11765,2.5);
#4649=CIRCLE('',#11767,2.5);
#4650=CIRCLE('',#11768,2.5);
#4651=CIRCLE('',#11770,2.5);
#4652=CIRCLE('',#11771,2.5);
#4653=CIRCLE('',#11773,10.);
#4654=CIRCLE('',#11774,10.);
#4655=CIRCLE('',#11777,1.5);
#4656=CIRCLE('',#11778,1.5);
#4657=CIRCLE('',#11781,1.5);
#4658=CIRCLE('',#11782,1.5);
#4659=CIRCLE('',#11785,1.5);
#4660=CIRCLE('',#11786,1.5);
#4661=CIRCLE('',#11789,1.5);
#4662=CIRCLE('',#11790,1.5);
#4663=CIRCLE('',#11792,2.5);
#4664=CIRCLE('',#11793,2.5);
#4665=CIRCLE('',#11795,2.5);
#4666=CIRCLE('',#11796,2.5);
#4667=CIRCLE('',#11798,2.5);
#4668=CIRCLE('',#11799,2.5);
#4669=CIRCLE('',#11801,2.5);
#4670=CIRCLE('',#11802,2.5);
#4671=CIRCLE('',#11804,10.);
#4672=CIRCLE('',#11805,10.);
#4673=CIRCLE('',#11808,1.5);
#4674=CIRCLE('',#11809,1.5);
#4675=CIRCLE('',#11812,1.5);
#4676=CIRCLE('',#11813,1.5);
#4677=CIRCLE('',#11816,1.5);
#4678=CIRCLE('',#11817,1.5);
#4679=CIRCLE('',#11820,1.5);
#4680=CIRCLE('',#11821,1.5);
#4681=CIRCLE('',#11823,2.5);
#4682=CIRCLE('',#11824,2.5);
#4683=CIRCLE('',#11826,2.5);
#4684=CIRCLE('',#11827,2.5);
#4685=CIRCLE('',#11829,2.5);
#4686=CIRCLE('',#11830,2.5);
#4687=CIRCLE('',#11832,2.5);
#4688=CIRCLE('',#11833,2.5);
#4689=CIRCLE('',#11835,10.);
#4690=CIRCLE('',#11836,10.);
#4691=CIRCLE('',#11839,1.5);
#4692=CIRCLE('',#11840,1.5);
#4693=CIRCLE('',#11843,1.5);
#4694=CIRCLE('',#11844,1.5);
#4695=CIRCLE('',#11847,1.5);
#4696=CIRCLE('',#11848,1.5);
#4697=CIRCLE('',#11851,1.5);
#4698=CIRCLE('',#11852,1.5);
#4699=CIRCLE('',#11854,2.5);
#4700=CIRCLE('',#11855,2.5);
#4701=CIRCLE('',#11857,2.5);
#4702=CIRCLE('',#11858,2.5);
#4703=CIRCLE('',#11860,2.5);
#4704=CIRCLE('',#11861,2.5);
#4705=CIRCLE('',#11863,2.5);
#4706=CIRCLE('',#11864,2.5);
#4707=CIRCLE('',#11866,10.);
#4708=CIRCLE('',#11867,10.);
#4709=CIRCLE('',#11870,1.5);
#4710=CIRCLE('',#11871,1.5);
#4711=CIRCLE('',#11874,1.5);
#4712=CIRCLE('',#11875,1.5);
#4713=CIRCLE('',#11878,1.5);
#4714=CIRCLE('',#11879,1.5);
#4715=CIRCLE('',#11882,1.5);
#4716=CIRCLE('',#11883,1.5);
#4717=CIRCLE('',#11885,2.5);
#4718=CIRCLE('',#11886,2.5);
#4719=CIRCLE('',#11888,2.5);
#4720=CIRCLE('',#11889,2.5);
#4721=CIRCLE('',#11891,2.5);
#4722=CIRCLE('',#11892,2.5);
#4723=CIRCLE('',#11894,2.5);
#4724=CIRCLE('',#11895,2.5);
#4725=CIRCLE('',#11897,10.);
#4726=CIRCLE('',#11898,10.);
#4727=CIRCLE('',#11901,1.5);
#4728=CIRCLE('',#11902,1.5);
#4729=CIRCLE('',#11905,1.5);
#4730=CIRCLE('',#11906,1.5);
#4731=CIRCLE('',#11909,1.5);
#4732=CIRCLE('',#11910,1.5);
#4733=CIRCLE('',#11913,1.5);
#4734=CIRCLE('',#11914,1.5);
#4735=CIRCLE('',#11916,2.5);
#4736=CIRCLE('',#11917,2.5);
#4737=CIRCLE('',#11919,2.5);
#4738=CIRCLE('',#11920,2.5);
#4739=CIRCLE('',#11922,2.5);
#4740=CIRCLE('',#11923,2.5);
#4741=CIRCLE('',#11925,2.5);
#4742=CIRCLE('',#11926,2.5);
#4743=CIRCLE('',#11928,10.);
#4744=CIRCLE('',#11929,10.);
#4745=CIRCLE('',#11932,1.5);
#4746=CIRCLE('',#11933,1.5);
#4747=CIRCLE('',#11936,1.5);
#4748=CIRCLE('',#11937,1.5);
#4749=CIRCLE('',#11940,1.5);
#4750=CIRCLE('',#11941,1.5);
#4751=CIRCLE('',#11944,1.5);
#4752=CIRCLE('',#11945,1.5);
#4753=CIRCLE('',#11947,2.5);
#4754=CIRCLE('',#11948,2.5);
#4755=CIRCLE('',#11950,2.5);
#4756=CIRCLE('',#11951,2.5);
#4757=CIRCLE('',#11953,2.5);
#4758=CIRCLE('',#11954,2.5);
#4759=CIRCLE('',#11956,2.5);
#4760=CIRCLE('',#11957,2.5);
#4761=CIRCLE('',#11959,10.);
#4762=CIRCLE('',#11960,10.);
#4763=CIRCLE('',#11963,1.5);
#4764=CIRCLE('',#11964,1.5);
#4765=CIRCLE('',#11967,1.5);
#4766=CIRCLE('',#11968,1.5);
#4767=CIRCLE('',#11971,1.5);
#4768=CIRCLE('',#11972,1.5);
#4769=CIRCLE('',#11975,1.5);
#4770=CIRCLE('',#11976,1.5);
#4771=CIRCLE('',#11978,2.5);
#4772=CIRCLE('',#11979,2.5);
#4773=CIRCLE('',#11981,2.5);
#4774=CIRCLE('',#11982,2.5);
#4775=CIRCLE('',#11984,2.5);
#4776=CIRCLE('',#11985,2.5);
#4777=CIRCLE('',#11987,2.5);
#4778=CIRCLE('',#11988,2.5);
#4779=CIRCLE('',#11990,10.);
#4780=CIRCLE('',#11991,10.);
#4781=CIRCLE('',#11994,1.5);
#4782=CIRCLE('',#11995,1.5);
#4783=CIRCLE('',#11998,1.5);
#4784=CIRCLE('',#11999,1.5);
#4785=CIRCLE('',#12002,1.5);
#4786=CIRCLE('',#12003,1.5);
#4787=CIRCLE('',#12006,1.5);
#4788=CIRCLE('',#12007,1.5);
#4789=CIRCLE('',#12009,2.5);
#4790=CIRCLE('',#12010,2.5);
#4791=CIRCLE('',#12012,2.5);
#4792=CIRCLE('',#12013,2.5);
#4793=CIRCLE('',#12015,2.5);
#4794=CIRCLE('',#12016,2.5);
#4795=CIRCLE('',#12018,2.5);
#4796=CIRCLE('',#12019,2.5);
#4797=CIRCLE('',#12021,10.);
#4798=CIRCLE('',#12022,10.);
#4799=CIRCLE('',#12025,1.5);
#4800=CIRCLE('',#12026,1.5);
#4801=CIRCLE('',#12029,1.5);
#4802=CIRCLE('',#12030,1.5);
#4803=CIRCLE('',#12033,1.5);
#4804=CIRCLE('',#12034,1.5);
#4805=CIRCLE('',#12037,1.5);
#4806=CIRCLE('',#12038,1.5);
#4807=CIRCLE('',#12040,2.5);
#4808=CIRCLE('',#12041,2.5);
#4809=CIRCLE('',#12043,2.5);
#4810=CIRCLE('',#12044,2.5);
#4811=CIRCLE('',#12047,1.5);
#4812=CIRCLE('',#12048,1.5);
#4813=CIRCLE('',#12051,1.5);
#4814=CIRCLE('',#12052,1.5);
#4815=CIRCLE('',#12055,1.5);
#4816=CIRCLE('',#12056,1.5);
#4817=CIRCLE('',#12059,1.5);
#4818=CIRCLE('',#12060,1.5);
#4819=CIRCLE('',#12062,10.);
#4820=CIRCLE('',#12063,10.);
#4821=CIRCLE('',#12065,2.5);
#4822=CIRCLE('',#12066,2.5);
#4823=CIRCLE('',#12068,2.5);
#4824=CIRCLE('',#12069,2.5);
#4825=CIRCLE('',#12071,0.5);
#4826=CIRCLE('',#12072,0.5);
#4827=CIRCLE('',#12075,0.5);
#4828=CIRCLE('',#12076,0.5);
#4829=CIRCLE('',#12078,2.);
#4830=CIRCLE('',#12079,1.99999999999999);
#4831=CIRCLE('',#12080,2.00000000000003);
#4832=CIRCLE('',#12081,1.99999999999999);
#4833=CIRCLE('',#12082,2.00000000000003);
#4834=CIRCLE('',#12083,2.);
#4835=CIRCLE('',#12084,1.99999999999999);
#4836=CIRCLE('',#12085,1.99999999999999);
#4837=CIRCLE('',#12086,1.99999999999999);
#4838=CIRCLE('',#12087,1.99999999999999);
#4839=CIRCLE('',#12088,1.99999999999999);
#4840=CIRCLE('',#12089,1.99999999999999);
#4841=CIRCLE('',#12090,2.);
#4842=CIRCLE('',#12091,1.99999999999999);
#4843=CIRCLE('',#12092,1.99999999999999);
#4844=CIRCLE('',#12093,1.99999999999999);
#4845=CIRCLE('',#12094,1.99999999999999);
#4846=CIRCLE('',#12095,2.);
#4847=CIRCLE('',#12096,2.);
#4848=CIRCLE('',#12097,2.00000000000003);
#4849=CIRCLE('',#12098,2.);
#4850=CIRCLE('',#12099,1.99999999999999);
#4851=CIRCLE('',#12100,2.);
#4852=CIRCLE('',#12101,1.99999999999999);
#4853=CIRCLE('',#12102,1.99999999999999);
#4854=CIRCLE('',#12103,1.99999999999999);
#4855=CIRCLE('',#12104,1.99999999999999);
#4856=CIRCLE('',#12105,1.99999999999999);
#4857=CIRCLE('',#12106,1.99999999999999);
#4858=CIRCLE('',#12107,1.99999999999999);
#4859=CIRCLE('',#12108,2.);
#4860=CIRCLE('',#12109,2.00000000000003);
#4861=CIRCLE('',#12110,1.99999999999999);
#4862=CIRCLE('',#12111,1.99999999999999);
#4863=CIRCLE('',#12112,1.99999999999999);
#4864=CIRCLE('',#12113,1.99999999999999);
#4865=CIRCLE('',#12114,2.);
#4866=CIRCLE('',#12115,2.00000000000003);
#4867=CIRCLE('',#12116,2.00000000000003);
#4868=CIRCLE('',#12117,2.00000000000003);
#4869=CIRCLE('',#12118,1.99999999999999);
#4870=CIRCLE('',#12119,1.99999999999999);
#4871=CIRCLE('',#12120,1.99999999999999);
#4872=CIRCLE('',#12121,2.00000000000003);
#4873=CIRCLE('',#12122,1.99999999999999);
#4874=CIRCLE('',#12123,1.99999999999999);
#4875=CIRCLE('',#12124,1.99999999999999);
#4876=CIRCLE('',#12126,2.);
#4877=CIRCLE('',#12127,2.);
#4878=CIRCLE('',#12130,2.);
#4879=CIRCLE('',#12132,2.);
#4880=CIRCLE('',#12134,2.);
#4881=CIRCLE('',#12136,1.99999999999999);
#4882=CIRCLE('',#12138,2.00000000000003);
#4883=CIRCLE('',#12140,1.99999999999999);
#4884=CIRCLE('',#12142,2.00000000000003);
#4885=CIRCLE('',#12144,2.);
#4886=CIRCLE('',#12146,1.99999999999999);
#4887=CIRCLE('',#12148,1.99999999999999);
#4888=CIRCLE('',#12150,1.99999999999999);
#4889=CIRCLE('',#12152,1.99999999999999);
#4890=CIRCLE('',#12154,1.99999999999999);
#4891=CIRCLE('',#12156,1.99999999999999);
#4892=CIRCLE('',#12158,2.);
#4893=CIRCLE('',#12160,1.99999999999999);
#4894=CIRCLE('',#12162,1.99999999999999);
#4895=CIRCLE('',#12164,1.99999999999999);
#4896=CIRCLE('',#12166,1.99999999999999);
#4897=CIRCLE('',#12168,2.);
#4898=CIRCLE('',#12170,2.);
#4899=CIRCLE('',#12172,2.00000000000003);
#4900=CIRCLE('',#12174,2.);
#4901=CIRCLE('',#12176,1.99999999999999);
#4902=CIRCLE('',#12178,2.);
#4903=CIRCLE('',#12180,1.99999999999999);
#4904=CIRCLE('',#12182,1.99999999999999);
#4905=CIRCLE('',#12184,1.99999999999999);
#4906=CIRCLE('',#12186,1.99999999999999);
#4907=CIRCLE('',#12188,1.99999999999999);
#4908=CIRCLE('',#12190,1.99999999999999);
#4909=CIRCLE('',#12192,1.99999999999999);
#4910=CIRCLE('',#12194,2.);
#4911=CIRCLE('',#12196,2.00000000000003);
#4912=CIRCLE('',#12198,1.99999999999999);
#4913=CIRCLE('',#12200,1.99999999999999);
#4914=CIRCLE('',#12202,1.99999999999999);
#4915=CIRCLE('',#12204,1.99999999999999);
#4916=CIRCLE('',#12206,2.);
#4917=CIRCLE('',#12208,2.00000000000003);
#4918=CIRCLE('',#12210,2.00000000000003);
#4919=CIRCLE('',#12212,2.00000000000003);
#4920=CIRCLE('',#12214,1.99999999999999);
#4921=CIRCLE('',#12216,1.99999999999999);
#4922=CIRCLE('',#12218,1.99999999999999);
#4923=CIRCLE('',#12220,2.00000000000003);
#4924=CIRCLE('',#12222,1.99999999999999);
#4925=CIRCLE('',#12224,1.99999999999999);
#4926=CIRCLE('',#12226,1.99999999999999);
#4927=CIRCLE('',#12230,2.);
#4928=CIRCLE('',#12231,2.);
#4929=CIRCLE('',#12233,1.99999999999999);
#4930=CIRCLE('',#12234,1.99999999999999);
#4931=CIRCLE('',#12236,2.00000000000003);
#4932=CIRCLE('',#12237,2.00000000000003);
#4933=CIRCLE('',#12239,1.99999999999999);
#4934=CIRCLE('',#12240,1.99999999999999);
#4935=CIRCLE('',#12242,2.00000000000003);
#4936=CIRCLE('',#12243,2.00000000000003);
#4937=CIRCLE('',#12245,2.);
#4938=CIRCLE('',#12246,2.);
#4939=CIRCLE('',#12248,1.99999999999999);
#4940=CIRCLE('',#12249,1.99999999999999);
#4941=CIRCLE('',#12251,1.99999999999999);
#4942=CIRCLE('',#12252,1.99999999999999);
#4943=CIRCLE('',#12254,1.99999999999999);
#4944=CIRCLE('',#12255,1.99999999999999);
#4945=CIRCLE('',#12257,1.99999999999999);
#4946=CIRCLE('',#12258,1.99999999999999);
#4947=CIRCLE('',#12260,1.99999999999999);
#4948=CIRCLE('',#12261,1.99999999999999);
#4949=CIRCLE('',#12263,1.99999999999999);
#4950=CIRCLE('',#12264,1.99999999999999);
#4951=CIRCLE('',#12266,2.);
#4952=CIRCLE('',#12267,2.);
#4953=CIRCLE('',#12269,1.99999999999999);
#4954=CIRCLE('',#12270,1.99999999999999);
#4955=CIRCLE('',#12272,1.99999999999999);
#4956=CIRCLE('',#12273,1.99999999999999);
#4957=CIRCLE('',#12275,1.99999999999999);
#4958=CIRCLE('',#12276,1.99999999999999);
#4959=CIRCLE('',#12278,1.99999999999999);
#4960=CIRCLE('',#12279,1.99999999999999);
#4961=CIRCLE('',#12281,2.);
#4962=CIRCLE('',#12282,2.);
#4963=CIRCLE('',#12284,2.);
#4964=CIRCLE('',#12285,2.);
#4965=CIRCLE('',#12287,2.00000000000003);
#4966=CIRCLE('',#12288,2.00000000000003);
#4967=CIRCLE('',#12290,2.);
#4968=CIRCLE('',#12291,2.);
#4969=CIRCLE('',#12293,1.99999999999999);
#4970=CIRCLE('',#12294,1.99999999999999);
#4971=CIRCLE('',#12296,2.);
#4972=CIRCLE('',#12297,2.);
#4973=CIRCLE('',#12299,1.99999999999999);
#4974=CIRCLE('',#12300,1.99999999999999);
#4975=CIRCLE('',#12302,1.99999999999999);
#4976=CIRCLE('',#12303,1.99999999999999);
#4977=CIRCLE('',#12305,1.99999999999999);
#4978=CIRCLE('',#12306,1.99999999999999);
#4979=CIRCLE('',#12308,1.99999999999999);
#4980=CIRCLE('',#12309,1.99999999999999);
#4981=CIRCLE('',#12311,1.99999999999999);
#4982=CIRCLE('',#12312,1.99999999999999);
#4983=CIRCLE('',#12314,1.99999999999999);
#4984=CIRCLE('',#12315,1.99999999999999);
#4985=CIRCLE('',#12317,1.99999999999999);
#4986=CIRCLE('',#12318,1.99999999999999);
#4987=CIRCLE('',#12320,2.);
#4988=CIRCLE('',#12321,2.);
#4989=CIRCLE('',#12323,2.00000000000003);
#4990=CIRCLE('',#12324,2.00000000000003);
#4991=CIRCLE('',#12326,1.99999999999999);
#4992=CIRCLE('',#12327,1.99999999999999);
#4993=CIRCLE('',#12329,1.99999999999999);
#4994=CIRCLE('',#12330,1.99999999999999);
#4995=CIRCLE('',#12332,1.99999999999999);
#4996=CIRCLE('',#12333,1.99999999999999);
#4997=CIRCLE('',#12335,1.99999999999999);
#4998=CIRCLE('',#12336,1.99999999999999);
#4999=CIRCLE('',#12338,2.);
#5000=CIRCLE('',#12339,2.);
#5001=CIRCLE('',#12341,2.00000000000003);
#5002=CIRCLE('',#12342,2.00000000000003);
#5003=CIRCLE('',#12344,2.00000000000003);
#5004=CIRCLE('',#12345,2.00000000000003);
#5005=CIRCLE('',#12347,2.00000000000003);
#5006=CIRCLE('',#12348,2.00000000000003);
#5007=CIRCLE('',#12350,1.99999999999999);
#5008=CIRCLE('',#12351,1.99999999999999);
#5009=CIRCLE('',#12353,1.99999999999999);
#5010=CIRCLE('',#12354,1.99999999999999);
#5011=CIRCLE('',#12356,1.99999999999999);
#5012=CIRCLE('',#12357,1.99999999999999);
#5013=CIRCLE('',#12359,2.00000000000003);
#5014=CIRCLE('',#12360,2.00000000000003);
#5015=CIRCLE('',#12362,1.99999999999999);
#5016=CIRCLE('',#12363,1.99999999999999);
#5017=CIRCLE('',#12365,1.99999999999999);
#5018=CIRCLE('',#12366,1.99999999999999);
#5019=CIRCLE('',#12368,1.99999999999999);
#5020=CIRCLE('',#12369,1.99999999999999);
#5021=CIRCLE('',#12376,1.49999999999999);
#5022=CIRCLE('',#12377,1.49999999999999);
#5023=CIRCLE('',#12379,2.00000000000003);
#5024=CIRCLE('',#12380,2.00000000000003);
#5025=CIRCLE('',#12382,2.00000000000003);
#5026=CIRCLE('',#12383,2.00000000000003);
#5027=CIRCLE('',#12385,2.);
#5028=CIRCLE('',#12386,2.);
#5029=CIRCLE('',#12388,1.49999999999999);
#5030=CIRCLE('',#12389,1.49999999999999);
#5031=CIRCLE('',#12390,1.49999999999999);
#5032=CIRCLE('',#12391,1.49999999999999);
#5033=CIRCLE('',#12392,1.49999999999999);
#5034=CIRCLE('',#12393,1.49999999999999);
#5035=CIRCLE('',#12394,1.49999999999999);
#5036=CIRCLE('',#12395,1.49999999999999);
#5037=CIRCLE('',#12396,1.49999999999999);
#5038=CIRCLE('',#12397,1.49999999999999);
#5039=CIRCLE('',#12398,1.49999999999999);
#5040=CIRCLE('',#12400,4.);
#5041=CIRCLE('',#12401,4.);
#5042=CIRCLE('',#12403,1.49999999999999);
#5043=CIRCLE('',#12404,1.49999999999999);
#5044=CIRCLE('',#12405,1.49999999999999);
#5045=CIRCLE('',#12406,1.49999999999999);
#5046=CIRCLE('',#12407,1.49999999999999);
#5047=CIRCLE('',#12408,1.49999999999999);
#5048=CIRCLE('',#12409,1.49999999999999);
#5049=CIRCLE('',#12410,1.49999999999999);
#5050=CIRCLE('',#12411,1.49999999999999);
#5051=CIRCLE('',#12412,1.49999999999999);
#5052=CIRCLE('',#12413,1.49999999999999);
#5053=CIRCLE('',#12431,1.49999999999999);
#5054=CIRCLE('',#12432,1.49999999999999);
#5055=CIRCLE('',#12433,1.49999999999999);
#5056=CIRCLE('',#12434,1.49999999999999);
#5057=CIRCLE('',#12435,1.49999999999999);
#5058=CIRCLE('',#12436,1.49999999999999);
#5059=CIRCLE('',#12437,1.49999999999999);
#5060=CIRCLE('',#12438,1.49999999999999);
#5061=CIRCLE('',#12439,1.49999999999999);
#5062=CIRCLE('',#12440,1.49999999999999);
#5063=CIRCLE('',#12441,1.49999999999999);
#5064=CIRCLE('',#12443,1.49999999999999);
#5065=CIRCLE('',#12445,1.49999999999999);
#5066=CIRCLE('',#12447,1.49999999999999);
#5067=CIRCLE('',#12449,1.49999999999999);
#5068=CIRCLE('',#12451,1.49999999999999);
#5069=CIRCLE('',#12453,1.49999999999999);
#5070=CIRCLE('',#12455,1.49999999999999);
#5071=CIRCLE('',#12457,1.49999999999999);
#5072=CIRCLE('',#12459,1.49999999999999);
#5073=CIRCLE('',#12461,1.49999999999999);
#5074=CIRCLE('',#12463,1.49999999999999);
#5075=CIRCLE('',#12478,1.465);
#5076=CIRCLE('',#12479,1.465);
#5077=CIRCLE('',#12490,1.5);
#5078=CIRCLE('',#12491,1.5);
#5079=CIRCLE('',#12493,2.00000000000003);
#5080=CIRCLE('',#12494,2.00000000000003);
#5081=CIRCLE('',#12496,2.00000000000003);
#5082=CIRCLE('',#12497,2.00000000000003);
#5083=CIRCLE('',#12499,2.);
#5084=CIRCLE('',#12500,2.);
#5085=CIRCLE('',#12502,1.49999999999999);
#5086=CIRCLE('',#12503,1.49999999999999);
#5087=CIRCLE('',#12504,1.49999999999999);
#5088=CIRCLE('',#12505,1.49999999999999);
#5089=CIRCLE('',#12506,1.49999999999999);
#5090=CIRCLE('',#12507,1.49999999999999);
#5091=CIRCLE('',#12508,1.49999999999999);
#5092=CIRCLE('',#12509,1.49999999999999);
#5093=CIRCLE('',#12510,1.49999999999999);
#5094=CIRCLE('',#12511,1.49999999999999);
#5095=CIRCLE('',#12512,1.49999999999999);
#5096=CIRCLE('',#12514,4.);
#5097=CIRCLE('',#12515,4.);
#5098=CIRCLE('',#12517,1.49999999999999);
#5099=CIRCLE('',#12518,1.49999999999999);
#5100=CIRCLE('',#12519,1.49999999999999);
#5101=CIRCLE('',#12520,1.49999999999999);
#5102=CIRCLE('',#12521,1.49999999999999);
#5103=CIRCLE('',#12522,1.49999999999999);
#5104=CIRCLE('',#12523,1.49999999999999);
#5105=CIRCLE('',#12524,1.49999999999999);
#5106=CIRCLE('',#12525,1.49999999999999);
#5107=CIRCLE('',#12526,1.49999999999999);
#5108=CIRCLE('',#12527,1.49999999999999);
#5109=CIRCLE('',#12545,1.49999999999999);
#5110=CIRCLE('',#12546,1.49999999999999);
#5111=CIRCLE('',#12547,1.49999999999999);
#5112=CIRCLE('',#12548,1.49999999999999);
#5113=CIRCLE('',#12549,1.49999999999999);
#5114=CIRCLE('',#12550,1.49999999999999);
#5115=CIRCLE('',#12551,1.49999999999999);
#5116=CIRCLE('',#12552,1.49999999999999);
#5117=CIRCLE('',#12553,1.49999999999999);
#5118=CIRCLE('',#12554,1.49999999999999);
#5119=CIRCLE('',#12555,1.49999999999999);
#5120=CIRCLE('',#12557,1.49999999999999);
#5121=CIRCLE('',#12559,1.49999999999999);
#5122=CIRCLE('',#12561,1.49999999999999);
#5123=CIRCLE('',#12563,1.49999999999999);
#5124=CIRCLE('',#12565,1.49999999999999);
#5125=CIRCLE('',#12567,1.49999999999999);
#5126=CIRCLE('',#12569,1.49999999999999);
#5127=CIRCLE('',#12571,1.49999999999999);
#5128=CIRCLE('',#12573,1.49999999999999);
#5129=CIRCLE('',#12575,1.49999999999999);
#5130=CIRCLE('',#12577,1.49999999999999);
#5131=CIRCLE('',#12592,1.4635);
#5132=CIRCLE('',#12601,1.4635);
#5133=CIRCLE('',#12605,1.465);
#5134=CIRCLE('',#12606,1.465);
#5135=CIRCLE('',#12617,1.465);
#5136=CIRCLE('',#12618,1.465);
#5137=CIRCLE('',#12630,0.999999999999975);
#5138=CIRCLE('',#12631,0.999999999999975);
#5139=CIRCLE('',#12635,1.99999999999998);
#5140=CIRCLE('',#12636,1.99999999999998);
#5141=CIRCLE('',#12639,0.500000000000007);
#5142=CIRCLE('',#12640,0.500000000000007);
#5143=CIRCLE('',#12642,0.499999999999998);
#5144=CIRCLE('',#12643,0.499999999999998);
#5145=CIRCLE('',#12647,0.999999999999975);
#5146=CIRCLE('',#12648,0.999999999999975);
#5147=CIRCLE('',#12652,1.99999999999998);
#5148=CIRCLE('',#12653,1.99999999999998);
#5149=CIRCLE('',#12656,0.500000000000007);
#5150=CIRCLE('',#12657,0.500000000000007);
#5151=CIRCLE('',#12660,0.499999999999998);
#5152=CIRCLE('',#12661,0.499999999999998);
#5153=CIRCLE('',#12666,0.999999999999981);
#5154=CIRCLE('',#12667,0.999999999999981);
#5155=CIRCLE('',#12670,0.999999999999967);
#5156=CIRCLE('',#12671,0.999999999999967);
#5157=CIRCLE('',#12676,1.99999999999997);
#5158=CIRCLE('',#12677,1.99999999999997);
#5159=CIRCLE('',#12680,1.99999999999998);
#5160=CIRCLE('',#12681,1.99999999999998);
#5161=CIRCLE('',#12684,0.999999999999981);
#5162=CIRCLE('',#12685,0.999999999999981);
#5163=CIRCLE('',#12688,0.999999999999967);
#5164=CIRCLE('',#12689,0.999999999999967);
#5165=CIRCLE('',#12694,1.99999999999997);
#5166=CIRCLE('',#12695,1.99999999999997);
#5167=CIRCLE('',#12698,1.99999999999998);
#5168=CIRCLE('',#12699,1.99999999999998);
#5169=CIRCLE('',#12704,1.465);
#5170=CIRCLE('',#12705,1.465);
#5171=VERTEX_POINT('',#16076);
#5172=VERTEX_POINT('',#16078);
#5173=VERTEX_POINT('',#16080);
#5174=VERTEX_POINT('',#16084);
#5175=VERTEX_POINT('',#16086);
#5176=VERTEX_POINT('',#16091);
#5177=VERTEX_POINT('',#16095);
#5178=VERTEX_POINT('',#16096);
#5179=VERTEX_POINT('',#16098);
#5180=VERTEX_POINT('',#16103);
#5181=VERTEX_POINT('',#16104);
#5182=VERTEX_POINT('',#16111);
#5183=VERTEX_POINT('',#16114);
#5184=VERTEX_POINT('',#16118);
#5185=VERTEX_POINT('',#16120);
#5186=VERTEX_POINT('',#16122);
#5187=VERTEX_POINT('',#16126);
#5188=VERTEX_POINT('',#16128);
#5189=VERTEX_POINT('',#16136);
#5190=VERTEX_POINT('',#16138);
#5191=VERTEX_POINT('',#16141);
#5192=VERTEX_POINT('',#16145);
#5193=VERTEX_POINT('',#16148);
#5194=VERTEX_POINT('',#16150);
#5195=VERTEX_POINT('',#16153);
#5196=VERTEX_POINT('',#16155);
#5197=VERTEX_POINT('',#16162);
#5198=VERTEX_POINT('',#16164);
#5199=VERTEX_POINT('',#16167);
#5200=VERTEX_POINT('',#16171);
#5201=VERTEX_POINT('',#16174);
#5202=VERTEX_POINT('',#16178);
#5203=VERTEX_POINT('',#16184);
#5204=VERTEX_POINT('',#16187);
#5205=VERTEX_POINT('',#16193);
#5206=VERTEX_POINT('',#16194);
#5207=VERTEX_POINT('',#16196);
#5208=VERTEX_POINT('',#16198);
#5209=VERTEX_POINT('',#16202);
#5210=VERTEX_POINT('',#16204);
#5211=VERTEX_POINT('',#16207);
#5212=VERTEX_POINT('',#16209);
#5213=VERTEX_POINT('',#16211);
#5214=VERTEX_POINT('',#16213);
#5215=VERTEX_POINT('',#16215);
#5216=VERTEX_POINT('',#16217);
#5217=VERTEX_POINT('',#16219);
#5218=VERTEX_POINT('',#16221);
#5219=VERTEX_POINT('',#16223);
#5220=VERTEX_POINT('',#16225);
#5221=VERTEX_POINT('',#16227);
#5222=VERTEX_POINT('',#16230);
#5223=VERTEX_POINT('',#16232);
#5224=VERTEX_POINT('',#16234);
#5225=VERTEX_POINT('',#16236);
#5226=VERTEX_POINT('',#16238);
#5227=VERTEX_POINT('',#16240);
#5228=VERTEX_POINT('',#16242);
#5229=VERTEX_POINT('',#16246);
#5230=VERTEX_POINT('',#16250);
#5231=VERTEX_POINT('',#16252);
#5232=VERTEX_POINT('',#16256);
#5233=VERTEX_POINT('',#16258);
#5234=VERTEX_POINT('',#16262);
#5235=VERTEX_POINT('',#16264);
#5236=VERTEX_POINT('',#16268);
#5237=VERTEX_POINT('',#16270);
#5238=VERTEX_POINT('',#16274);
#5239=VERTEX_POINT('',#16276);
#5240=VERTEX_POINT('',#16280);
#5241=VERTEX_POINT('',#16282);
#5242=VERTEX_POINT('',#16286);
#5243=VERTEX_POINT('',#16288);
#5244=VERTEX_POINT('',#16292);
#5245=VERTEX_POINT('',#16294);
#5246=VERTEX_POINT('',#16298);
#5247=VERTEX_POINT('',#16300);
#5248=VERTEX_POINT('',#16304);
#5249=VERTEX_POINT('',#16306);
#5250=VERTEX_POINT('',#16310);
#5251=VERTEX_POINT('',#16312);
#5252=VERTEX_POINT('',#16316);
#5253=VERTEX_POINT('',#16320);
#5254=VERTEX_POINT('',#16324);
#5255=VERTEX_POINT('',#16328);
#5256=VERTEX_POINT('',#16332);
#5257=VERTEX_POINT('',#16336);
#5258=VERTEX_POINT('',#16340);
#5259=VERTEX_POINT('',#16344);
#5260=VERTEX_POINT('',#16348);
#5261=VERTEX_POINT('',#16352);
#5262=VERTEX_POINT('',#16356);
#5263=VERTEX_POINT('',#16360);
#5264=VERTEX_POINT('',#16362);
#5265=VERTEX_POINT('',#16366);
#5266=VERTEX_POINT('',#16368);
#5267=VERTEX_POINT('',#16372);
#5268=VERTEX_POINT('',#16374);
#5269=VERTEX_POINT('',#16378);
#5270=VERTEX_POINT('',#16380);
#5271=VERTEX_POINT('',#16384);
#5272=VERTEX_POINT('',#16386);
#5273=VERTEX_POINT('',#16390);
#5274=VERTEX_POINT('',#16392);
#5275=VERTEX_POINT('',#16396);
#5276=VERTEX_POINT('',#16398);
#5277=VERTEX_POINT('',#16402);
#5278=VERTEX_POINT('',#16404);
#5279=VERTEX_POINT('',#16408);
#5280=VERTEX_POINT('',#16410);
#5281=VERTEX_POINT('',#16414);
#5282=VERTEX_POINT('',#16416);
#5283=VERTEX_POINT('',#16420);
#5284=VERTEX_POINT('',#16422);
#5285=VERTEX_POINT('',#16426);
#5286=VERTEX_POINT('',#16428);
#5287=VERTEX_POINT('',#16434);
#5288=VERTEX_POINT('',#16438);
#5289=VERTEX_POINT('',#16442);
#5290=VERTEX_POINT('',#16446);
#5291=VERTEX_POINT('',#16454);
#5292=VERTEX_POINT('',#16455);
#5293=VERTEX_POINT('',#16457);
#5294=VERTEX_POINT('',#16459);
#5295=VERTEX_POINT('',#16461);
#5296=VERTEX_POINT('',#16463);
#5297=VERTEX_POINT('',#16466);
#5298=VERTEX_POINT('',#16469);
#5299=VERTEX_POINT('',#16471);
#5300=VERTEX_POINT('',#16475);
#5301=VERTEX_POINT('',#16479);
#5302=VERTEX_POINT('',#16483);
#5303=VERTEX_POINT('',#16487);
#5304=VERTEX_POINT('',#16494);
#5305=VERTEX_POINT('',#16500);
#5306=VERTEX_POINT('',#16501);
#5307=VERTEX_POINT('',#16503);
#5308=VERTEX_POINT('',#16505);
#5309=VERTEX_POINT('',#16509);
#5310=VERTEX_POINT('',#16511);
#5311=VERTEX_POINT('',#16515);
#5312=VERTEX_POINT('',#16517);
#5313=VERTEX_POINT('',#16521);
#5314=VERTEX_POINT('',#16522);
#5315=VERTEX_POINT('',#16524);
#5316=VERTEX_POINT('',#16526);
#5317=VERTEX_POINT('',#16530);
#5318=VERTEX_POINT('',#16532);
#5319=VERTEX_POINT('',#16536);
#5320=VERTEX_POINT('',#16538);
#5321=VERTEX_POINT('',#16542);
#5322=VERTEX_POINT('',#16544);
#5323=VERTEX_POINT('',#16548);
#5324=VERTEX_POINT('',#16550);
#5325=VERTEX_POINT('',#16554);
#5326=VERTEX_POINT('',#16556);
#5327=VERTEX_POINT('',#16560);
#5328=VERTEX_POINT('',#16561);
#5329=VERTEX_POINT('',#16563);
#5330=VERTEX_POINT('',#16565);
#5331=VERTEX_POINT('',#16569);
#5332=VERTEX_POINT('',#16571);
#5333=VERTEX_POINT('',#16575);
#5334=VERTEX_POINT('',#16577);
#5335=VERTEX_POINT('',#16581);
#5336=VERTEX_POINT('',#16582);
#5337=VERTEX_POINT('',#16584);
#5338=VERTEX_POINT('',#16586);
#5339=VERTEX_POINT('',#16590);
#5340=VERTEX_POINT('',#16592);
#5341=VERTEX_POINT('',#16596);
#5342=VERTEX_POINT('',#16598);
#5343=VERTEX_POINT('',#16605);
#5344=VERTEX_POINT('',#16607);
#5345=VERTEX_POINT('',#16614);
#5346=VERTEX_POINT('',#16616);
#5347=VERTEX_POINT('',#16620);
#5348=VERTEX_POINT('',#16622);
#5349=VERTEX_POINT('',#16629);
#5350=VERTEX_POINT('',#16631);
#5351=VERTEX_POINT('',#16635);
#5352=VERTEX_POINT('',#16637);
#5353=VERTEX_POINT('',#16641);
#5354=VERTEX_POINT('',#16643);
#5355=VERTEX_POINT('',#16647);
#5356=VERTEX_POINT('',#16649);
#5357=VERTEX_POINT('',#16653);
#5358=VERTEX_POINT('',#16655);
#5359=VERTEX_POINT('',#16659);
#5360=VERTEX_POINT('',#16661);
#5361=VERTEX_POINT('',#16665);
#5362=VERTEX_POINT('',#16667);
#5363=VERTEX_POINT('',#16671);
#5364=VERTEX_POINT('',#16673);
#5365=VERTEX_POINT('',#16677);
#5366=VERTEX_POINT('',#16679);
#5367=VERTEX_POINT('',#16683);
#5368=VERTEX_POINT('',#16685);
#5369=VERTEX_POINT('',#16689);
#5370=VERTEX_POINT('',#16691);
#5371=VERTEX_POINT('',#16695);
#5372=VERTEX_POINT('',#16697);
#5373=VERTEX_POINT('',#16701);
#5374=VERTEX_POINT('',#16703);
#5375=VERTEX_POINT('',#16707);
#5376=VERTEX_POINT('',#16709);
#5377=VERTEX_POINT('',#16713);
#5378=VERTEX_POINT('',#16715);
#5379=VERTEX_POINT('',#16719);
#5380=VERTEX_POINT('',#16721);
#5381=VERTEX_POINT('',#16725);
#5382=VERTEX_POINT('',#16727);
#5383=VERTEX_POINT('',#16731);
#5384=VERTEX_POINT('',#16733);
#5385=VERTEX_POINT('',#16743);
#5386=VERTEX_POINT('',#16745);
#5387=VERTEX_POINT('',#16749);
#5388=VERTEX_POINT('',#16751);
#5389=VERTEX_POINT('',#16755);
#5390=VERTEX_POINT('',#16757);
#5391=VERTEX_POINT('',#16761);
#5392=VERTEX_POINT('',#16763);
#5393=VERTEX_POINT('',#16767);
#5394=VERTEX_POINT('',#16769);
#5395=VERTEX_POINT('',#16773);
#5396=VERTEX_POINT('',#16774);
#5397=VERTEX_POINT('',#16776);
#5398=VERTEX_POINT('',#16778);
#5399=VERTEX_POINT('',#16782);
#5400=VERTEX_POINT('',#16784);
#5401=VERTEX_POINT('',#16788);
#5402=VERTEX_POINT('',#16790);
#5403=VERTEX_POINT('',#16797);
#5404=VERTEX_POINT('',#16798);
#5405=VERTEX_POINT('',#16800);
#5406=VERTEX_POINT('',#16802);
#5407=VERTEX_POINT('',#16806);
#5408=VERTEX_POINT('',#16808);
#5409=VERTEX_POINT('',#16812);
#5410=VERTEX_POINT('',#16814);
#5411=VERTEX_POINT('',#16821);
#5412=VERTEX_POINT('',#16823);
#5413=VERTEX_POINT('',#16827);
#5414=VERTEX_POINT('',#16829);
#5415=VERTEX_POINT('',#16833);
#5416=VERTEX_POINT('',#16835);
#5417=VERTEX_POINT('',#16839);
#5418=VERTEX_POINT('',#16841);
#5419=VERTEX_POINT('',#16845);
#5420=VERTEX_POINT('',#16847);
#5421=VERTEX_POINT('',#16851);
#5422=VERTEX_POINT('',#16852);
#5423=VERTEX_POINT('',#16854);
#5424=VERTEX_POINT('',#16856);
#5425=VERTEX_POINT('',#16860);
#5426=VERTEX_POINT('',#16862);
#5427=VERTEX_POINT('',#16866);
#5428=VERTEX_POINT('',#16868);
#5429=VERTEX_POINT('',#16875);
#5430=VERTEX_POINT('',#16876);
#5431=VERTEX_POINT('',#16878);
#5432=VERTEX_POINT('',#16880);
#5433=VERTEX_POINT('',#16884);
#5434=VERTEX_POINT('',#16886);
#5435=VERTEX_POINT('',#16890);
#5436=VERTEX_POINT('',#16892);
#5437=VERTEX_POINT('',#16899);
#5438=VERTEX_POINT('',#16901);
#5439=VERTEX_POINT('',#16905);
#5440=VERTEX_POINT('',#16907);
#5441=VERTEX_POINT('',#16911);
#5442=VERTEX_POINT('',#16913);
#5443=VERTEX_POINT('',#16917);
#5444=VERTEX_POINT('',#16919);
#5445=VERTEX_POINT('',#16923);
#5446=VERTEX_POINT('',#16925);
#5447=VERTEX_POINT('',#16929);
#5448=VERTEX_POINT('',#16930);
#5449=VERTEX_POINT('',#16932);
#5450=VERTEX_POINT('',#16934);
#5451=VERTEX_POINT('',#16938);
#5452=VERTEX_POINT('',#16940);
#5453=VERTEX_POINT('',#16944);
#5454=VERTEX_POINT('',#16946);
#5455=VERTEX_POINT('',#16953);
#5456=VERTEX_POINT('',#16954);
#5457=VERTEX_POINT('',#16956);
#5458=VERTEX_POINT('',#16958);
#5459=VERTEX_POINT('',#16962);
#5460=VERTEX_POINT('',#16964);
#5461=VERTEX_POINT('',#16968);
#5462=VERTEX_POINT('',#16970);
#5463=VERTEX_POINT('',#16977);
#5464=VERTEX_POINT('',#16979);
#5465=VERTEX_POINT('',#16983);
#5466=VERTEX_POINT('',#16985);
#5467=VERTEX_POINT('',#16989);
#5468=VERTEX_POINT('',#16991);
#5469=VERTEX_POINT('',#16995);
#5470=VERTEX_POINT('',#16997);
#5471=VERTEX_POINT('',#17001);
#5472=VERTEX_POINT('',#17003);
#5473=VERTEX_POINT('',#17007);
#5474=VERTEX_POINT('',#17008);
#5475=VERTEX_POINT('',#17010);
#5476=VERTEX_POINT('',#17012);
#5477=VERTEX_POINT('',#17016);
#5478=VERTEX_POINT('',#17018);
#5479=VERTEX_POINT('',#17022);
#5480=VERTEX_POINT('',#17024);
#5481=VERTEX_POINT('',#17031);
#5482=VERTEX_POINT('',#17032);
#5483=VERTEX_POINT('',#17034);
#5484=VERTEX_POINT('',#17036);
#5485=VERTEX_POINT('',#17040);
#5486=VERTEX_POINT('',#17042);
#5487=VERTEX_POINT('',#17046);
#5488=VERTEX_POINT('',#17048);
#5489=VERTEX_POINT('',#17055);
#5490=VERTEX_POINT('',#17057);
#5491=VERTEX_POINT('',#17061);
#5492=VERTEX_POINT('',#17063);
#5493=VERTEX_POINT('',#17067);
#5494=VERTEX_POINT('',#17069);
#5495=VERTEX_POINT('',#17073);
#5496=VERTEX_POINT('',#17075);
#5497=VERTEX_POINT('',#17079);
#5498=VERTEX_POINT('',#17081);
#5499=VERTEX_POINT('',#17085);
#5500=VERTEX_POINT('',#17086);
#5501=VERTEX_POINT('',#17088);
#5502=VERTEX_POINT('',#17090);
#5503=VERTEX_POINT('',#17094);
#5504=VERTEX_POINT('',#17096);
#5505=VERTEX_POINT('',#17100);
#5506=VERTEX_POINT('',#17102);
#5507=VERTEX_POINT('',#17109);
#5508=VERTEX_POINT('',#17110);
#5509=VERTEX_POINT('',#17112);
#5510=VERTEX_POINT('',#17114);
#5511=VERTEX_POINT('',#17118);
#5512=VERTEX_POINT('',#17120);
#5513=VERTEX_POINT('',#17124);
#5514=VERTEX_POINT('',#17126);
#5515=VERTEX_POINT('',#17133);
#5516=VERTEX_POINT('',#17135);
#5517=VERTEX_POINT('',#17139);
#5518=VERTEX_POINT('',#17141);
#5519=VERTEX_POINT('',#17145);
#5520=VERTEX_POINT('',#17147);
#5521=VERTEX_POINT('',#17151);
#5522=VERTEX_POINT('',#17153);
#5523=VERTEX_POINT('',#17157);
#5524=VERTEX_POINT('',#17159);
#5525=VERTEX_POINT('',#17163);
#5526=VERTEX_POINT('',#17164);
#5527=VERTEX_POINT('',#17166);
#5528=VERTEX_POINT('',#17168);
#5529=VERTEX_POINT('',#17172);
#5530=VERTEX_POINT('',#17174);
#5531=VERTEX_POINT('',#17178);
#5532=VERTEX_POINT('',#17180);
#5533=VERTEX_POINT('',#17187);
#5534=VERTEX_POINT('',#17188);
#5535=VERTEX_POINT('',#17190);
#5536=VERTEX_POINT('',#17192);
#5537=VERTEX_POINT('',#17196);
#5538=VERTEX_POINT('',#17198);
#5539=VERTEX_POINT('',#17202);
#5540=VERTEX_POINT('',#17204);
#5541=VERTEX_POINT('',#17211);
#5542=VERTEX_POINT('',#17213);
#5543=VERTEX_POINT('',#17217);
#5544=VERTEX_POINT('',#17219);
#5545=VERTEX_POINT('',#17223);
#5546=VERTEX_POINT('',#17225);
#5547=VERTEX_POINT('',#17229);
#5548=VERTEX_POINT('',#17231);
#5549=VERTEX_POINT('',#17235);
#5550=VERTEX_POINT('',#17237);
#5551=VERTEX_POINT('',#17241);
#5552=VERTEX_POINT('',#17242);
#5553=VERTEX_POINT('',#17244);
#5554=VERTEX_POINT('',#17246);
#5555=VERTEX_POINT('',#17250);
#5556=VERTEX_POINT('',#17252);
#5557=VERTEX_POINT('',#17256);
#5558=VERTEX_POINT('',#17258);
#5559=VERTEX_POINT('',#17265);
#5560=VERTEX_POINT('',#17266);
#5561=VERTEX_POINT('',#17268);
#5562=VERTEX_POINT('',#17270);
#5563=VERTEX_POINT('',#17274);
#5564=VERTEX_POINT('',#17276);
#5565=VERTEX_POINT('',#17280);
#5566=VERTEX_POINT('',#17282);
#5567=VERTEX_POINT('',#17289);
#5568=VERTEX_POINT('',#17291);
#5569=VERTEX_POINT('',#17295);
#5570=VERTEX_POINT('',#17297);
#5571=VERTEX_POINT('',#17301);
#5572=VERTEX_POINT('',#17303);
#5573=VERTEX_POINT('',#17307);
#5574=VERTEX_POINT('',#17309);
#5575=VERTEX_POINT('',#17313);
#5576=VERTEX_POINT('',#17315);
#5577=VERTEX_POINT('',#17319);
#5578=VERTEX_POINT('',#17320);
#5579=VERTEX_POINT('',#17322);
#5580=VERTEX_POINT('',#17324);
#5581=VERTEX_POINT('',#17328);
#5582=VERTEX_POINT('',#17330);
#5583=VERTEX_POINT('',#17334);
#5584=VERTEX_POINT('',#17336);
#5585=VERTEX_POINT('',#17343);
#5586=VERTEX_POINT('',#17344);
#5587=VERTEX_POINT('',#17346);
#5588=VERTEX_POINT('',#17348);
#5589=VERTEX_POINT('',#17352);
#5590=VERTEX_POINT('',#17354);
#5591=VERTEX_POINT('',#17358);
#5592=VERTEX_POINT('',#17360);
#5593=VERTEX_POINT('',#17367);
#5594=VERTEX_POINT('',#17369);
#5595=VERTEX_POINT('',#17373);
#5596=VERTEX_POINT('',#17375);
#5597=VERTEX_POINT('',#17379);
#5598=VERTEX_POINT('',#17381);
#5599=VERTEX_POINT('',#17385);
#5600=VERTEX_POINT('',#17387);
#5601=VERTEX_POINT('',#17391);
#5602=VERTEX_POINT('',#17393);
#5603=VERTEX_POINT('',#17397);
#5604=VERTEX_POINT('',#17398);
#5605=VERTEX_POINT('',#17400);
#5606=VERTEX_POINT('',#17402);
#5607=VERTEX_POINT('',#17406);
#5608=VERTEX_POINT('',#17408);
#5609=VERTEX_POINT('',#17412);
#5610=VERTEX_POINT('',#17414);
#5611=VERTEX_POINT('',#17421);
#5612=VERTEX_POINT('',#17422);
#5613=VERTEX_POINT('',#17424);
#5614=VERTEX_POINT('',#17426);
#5615=VERTEX_POINT('',#17430);
#5616=VERTEX_POINT('',#17432);
#5617=VERTEX_POINT('',#17436);
#5618=VERTEX_POINT('',#17438);
#5619=VERTEX_POINT('',#17445);
#5620=VERTEX_POINT('',#17447);
#5621=VERTEX_POINT('',#17451);
#5622=VERTEX_POINT('',#17453);
#5623=VERTEX_POINT('',#17457);
#5624=VERTEX_POINT('',#17458);
#5625=VERTEX_POINT('',#17460);
#5626=VERTEX_POINT('',#17462);
#5627=VERTEX_POINT('',#17466);
#5628=VERTEX_POINT('',#17468);
#5629=VERTEX_POINT('',#17472);
#5630=VERTEX_POINT('',#17474);
#5631=VERTEX_POINT('',#17481);
#5632=VERTEX_POINT('',#17482);
#5633=VERTEX_POINT('',#17484);
#5634=VERTEX_POINT('',#17486);
#5635=VERTEX_POINT('',#17490);
#5636=VERTEX_POINT('',#17492);
#5637=VERTEX_POINT('',#17496);
#5638=VERTEX_POINT('',#17498);
#5639=VERTEX_POINT('',#17505);
#5640=VERTEX_POINT('',#17507);
#5641=VERTEX_POINT('',#17511);
#5642=VERTEX_POINT('',#17513);
#5643=VERTEX_POINT('',#17517);
#5644=VERTEX_POINT('',#17519);
#5645=VERTEX_POINT('',#17523);
#5646=VERTEX_POINT('',#17524);
#5647=VERTEX_POINT('',#17526);
#5648=VERTEX_POINT('',#17528);
#5649=VERTEX_POINT('',#17532);
#5650=VERTEX_POINT('',#17534);
#5651=VERTEX_POINT('',#17538);
#5652=VERTEX_POINT('',#17540);
#5653=VERTEX_POINT('',#17544);
#5654=VERTEX_POINT('',#17546);
#5655=VERTEX_POINT('',#17549);
#5656=VERTEX_POINT('',#17551);
#5657=VERTEX_POINT('',#17553);
#5658=VERTEX_POINT('',#17555);
#5659=VERTEX_POINT('',#17557);
#5660=VERTEX_POINT('',#17559);
#5661=VERTEX_POINT('',#17561);
#5662=VERTEX_POINT('',#17563);
#5663=VERTEX_POINT('',#17565);
#5664=VERTEX_POINT('',#17567);
#5665=VERTEX_POINT('',#17569);
#5666=VERTEX_POINT('',#17571);
#5667=VERTEX_POINT('',#17573);
#5668=VERTEX_POINT('',#17575);
#5669=VERTEX_POINT('',#17577);
#5670=VERTEX_POINT('',#17579);
#5671=VERTEX_POINT('',#17581);
#5672=VERTEX_POINT('',#17583);
#5673=VERTEX_POINT('',#17585);
#5674=VERTEX_POINT('',#17587);
#5675=VERTEX_POINT('',#17589);
#5676=VERTEX_POINT('',#17591);
#5677=VERTEX_POINT('',#17593);
#5678=VERTEX_POINT('',#17595);
#5679=VERTEX_POINT('',#17597);
#5680=VERTEX_POINT('',#17599);
#5681=VERTEX_POINT('',#17601);
#5682=VERTEX_POINT('',#17603);
#5683=VERTEX_POINT('',#17605);
#5684=VERTEX_POINT('',#17607);
#5685=VERTEX_POINT('',#17609);
#5686=VERTEX_POINT('',#17611);
#5687=VERTEX_POINT('',#17613);
#5688=VERTEX_POINT('',#17615);
#5689=VERTEX_POINT('',#17617);
#5690=VERTEX_POINT('',#17619);
#5691=VERTEX_POINT('',#17621);
#5692=VERTEX_POINT('',#17623);
#5693=VERTEX_POINT('',#17625);
#5694=VERTEX_POINT('',#17627);
#5695=VERTEX_POINT('',#17629);
#5696=VERTEX_POINT('',#17631);
#5697=VERTEX_POINT('',#17633);
#5698=VERTEX_POINT('',#17635);
#5699=VERTEX_POINT('',#17637);
#5700=VERTEX_POINT('',#17639);
#5701=VERTEX_POINT('',#17641);
#5702=VERTEX_POINT('',#17644);
#5703=VERTEX_POINT('',#17645);
#5704=VERTEX_POINT('',#17647);
#5705=VERTEX_POINT('',#17649);
#5706=VERTEX_POINT('',#17653);
#5707=VERTEX_POINT('',#17655);
#5708=VERTEX_POINT('',#17659);
#5709=VERTEX_POINT('',#17662);
#5710=VERTEX_POINT('',#17664);
#5711=VERTEX_POINT('',#17666);
#5712=VERTEX_POINT('',#17670);
#5713=VERTEX_POINT('',#17674);
#5714=VERTEX_POINT('',#17678);
#5715=VERTEX_POINT('',#17682);
#5716=VERTEX_POINT('',#17686);
#5717=VERTEX_POINT('',#17690);
#5718=VERTEX_POINT('',#17694);
#5719=VERTEX_POINT('',#17698);
#5720=VERTEX_POINT('',#17702);
#5721=VERTEX_POINT('',#17706);
#5722=VERTEX_POINT('',#17710);
#5723=VERTEX_POINT('',#17714);
#5724=VERTEX_POINT('',#17718);
#5725=VERTEX_POINT('',#17722);
#5726=VERTEX_POINT('',#17726);
#5727=VERTEX_POINT('',#17730);
#5728=VERTEX_POINT('',#17734);
#5729=VERTEX_POINT('',#17738);
#5730=VERTEX_POINT('',#17742);
#5731=VERTEX_POINT('',#17746);
#5732=VERTEX_POINT('',#17750);
#5733=VERTEX_POINT('',#17754);
#5734=VERTEX_POINT('',#17758);
#5735=VERTEX_POINT('',#17762);
#5736=VERTEX_POINT('',#17766);
#5737=VERTEX_POINT('',#17770);
#5738=VERTEX_POINT('',#17774);
#5739=VERTEX_POINT('',#17778);
#5740=VERTEX_POINT('',#17782);
#5741=VERTEX_POINT('',#17786);
#5742=VERTEX_POINT('',#17790);
#5743=VERTEX_POINT('',#17794);
#5744=VERTEX_POINT('',#17798);
#5745=VERTEX_POINT('',#17802);
#5746=VERTEX_POINT('',#17806);
#5747=VERTEX_POINT('',#17810);
#5748=VERTEX_POINT('',#17814);
#5749=VERTEX_POINT('',#17818);
#5750=VERTEX_POINT('',#17822);
#5751=VERTEX_POINT('',#17826);
#5752=VERTEX_POINT('',#17830);
#5753=VERTEX_POINT('',#17834);
#5754=VERTEX_POINT('',#17838);
#5755=VERTEX_POINT('',#17842);
#5756=VERTEX_POINT('',#17846);
#5757=VERTEX_POINT('',#17850);
#5758=VERTEX_POINT('',#17854);
#5759=VERTEX_POINT('',#17858);
#5760=VERTEX_POINT('',#17862);
#5761=VERTEX_POINT('',#17868);
#5762=VERTEX_POINT('',#17870);
#5763=VERTEX_POINT('',#17874);
#5764=VERTEX_POINT('',#17876);
#5765=VERTEX_POINT('',#17880);
#5766=VERTEX_POINT('',#17882);
#5767=VERTEX_POINT('',#17886);
#5768=VERTEX_POINT('',#17888);
#5769=VERTEX_POINT('',#17892);
#5770=VERTEX_POINT('',#17894);
#5771=VERTEX_POINT('',#17898);
#5772=VERTEX_POINT('',#17900);
#5773=VERTEX_POINT('',#17904);
#5774=VERTEX_POINT('',#17906);
#5775=VERTEX_POINT('',#17910);
#5776=VERTEX_POINT('',#17912);
#5777=VERTEX_POINT('',#17916);
#5778=VERTEX_POINT('',#17918);
#5779=VERTEX_POINT('',#17922);
#5780=VERTEX_POINT('',#17924);
#5781=VERTEX_POINT('',#17928);
#5782=VERTEX_POINT('',#17930);
#5783=VERTEX_POINT('',#17934);
#5784=VERTEX_POINT('',#17936);
#5785=VERTEX_POINT('',#17940);
#5786=VERTEX_POINT('',#17942);
#5787=VERTEX_POINT('',#17946);
#5788=VERTEX_POINT('',#17948);
#5789=VERTEX_POINT('',#17952);
#5790=VERTEX_POINT('',#17954);
#5791=VERTEX_POINT('',#17958);
#5792=VERTEX_POINT('',#17960);
#5793=VERTEX_POINT('',#17964);
#5794=VERTEX_POINT('',#17966);
#5795=VERTEX_POINT('',#17970);
#5796=VERTEX_POINT('',#17972);
#5797=VERTEX_POINT('',#17976);
#5798=VERTEX_POINT('',#17978);
#5799=VERTEX_POINT('',#17982);
#5800=VERTEX_POINT('',#17984);
#5801=VERTEX_POINT('',#17988);
#5802=VERTEX_POINT('',#17990);
#5803=VERTEX_POINT('',#17994);
#5804=VERTEX_POINT('',#17996);
#5805=VERTEX_POINT('',#18000);
#5806=VERTEX_POINT('',#18002);
#5807=VERTEX_POINT('',#18006);
#5808=VERTEX_POINT('',#18008);
#5809=VERTEX_POINT('',#18012);
#5810=VERTEX_POINT('',#18014);
#5811=VERTEX_POINT('',#18018);
#5812=VERTEX_POINT('',#18020);
#5813=VERTEX_POINT('',#18024);
#5814=VERTEX_POINT('',#18026);
#5815=VERTEX_POINT('',#18030);
#5816=VERTEX_POINT('',#18032);
#5817=VERTEX_POINT('',#18036);
#5818=VERTEX_POINT('',#18038);
#5819=VERTEX_POINT('',#18042);
#5820=VERTEX_POINT('',#18044);
#5821=VERTEX_POINT('',#18048);
#5822=VERTEX_POINT('',#18050);
#5823=VERTEX_POINT('',#18054);
#5824=VERTEX_POINT('',#18056);
#5825=VERTEX_POINT('',#18060);
#5826=VERTEX_POINT('',#18062);
#5827=VERTEX_POINT('',#18066);
#5828=VERTEX_POINT('',#18068);
#5829=VERTEX_POINT('',#18072);
#5830=VERTEX_POINT('',#18074);
#5831=VERTEX_POINT('',#18078);
#5832=VERTEX_POINT('',#18080);
#5833=VERTEX_POINT('',#18084);
#5834=VERTEX_POINT('',#18086);
#5835=VERTEX_POINT('',#18090);
#5836=VERTEX_POINT('',#18092);
#5837=VERTEX_POINT('',#18096);
#5838=VERTEX_POINT('',#18098);
#5839=VERTEX_POINT('',#18102);
#5840=VERTEX_POINT('',#18104);
#5841=VERTEX_POINT('',#18108);
#5842=VERTEX_POINT('',#18110);
#5843=VERTEX_POINT('',#18114);
#5844=VERTEX_POINT('',#18116);
#5845=VERTEX_POINT('',#18120);
#5846=VERTEX_POINT('',#18122);
#5847=VERTEX_POINT('',#18126);
#5848=VERTEX_POINT('',#18128);
#5849=VERTEX_POINT('',#18132);
#5850=VERTEX_POINT('',#18134);
#5851=VERTEX_POINT('',#18138);
#5852=VERTEX_POINT('',#18140);
#5853=VERTEX_POINT('',#18144);
#5854=VERTEX_POINT('',#18146);
#5855=VERTEX_POINT('',#18150);
#5856=VERTEX_POINT('',#18152);
#5857=VERTEX_POINT('',#18162);
#5858=VERTEX_POINT('',#18164);
#5859=VERTEX_POINT('',#18168);
#5860=VERTEX_POINT('',#18170);
#5861=VERTEX_POINT('',#18174);
#5862=VERTEX_POINT('',#18176);
#5863=VERTEX_POINT('',#18180);
#5864=VERTEX_POINT('',#18181);
#5865=VERTEX_POINT('',#18183);
#5866=VERTEX_POINT('',#18185);
#5867=VERTEX_POINT('',#18189);
#5868=VERTEX_POINT('',#18191);
#5869=VERTEX_POINT('',#18193);
#5870=VERTEX_POINT('',#18195);
#5871=VERTEX_POINT('',#18197);
#5872=VERTEX_POINT('',#18199);
#5873=VERTEX_POINT('',#18202);
#5874=VERTEX_POINT('',#18204);
#5875=VERTEX_POINT('',#18206);
#5876=VERTEX_POINT('',#18208);
#5877=VERTEX_POINT('',#18210);
#5878=VERTEX_POINT('',#18212);
#5879=VERTEX_POINT('',#18214);
#5880=VERTEX_POINT('',#18216);
#5881=VERTEX_POINT('',#18218);
#5882=VERTEX_POINT('',#18220);
#5883=VERTEX_POINT('',#18222);
#5884=VERTEX_POINT('',#18225);
#5885=VERTEX_POINT('',#18226);
#5886=VERTEX_POINT('',#18228);
#5887=VERTEX_POINT('',#18230);
#5888=VERTEX_POINT('',#18234);
#5889=VERTEX_POINT('',#18236);
#5890=VERTEX_POINT('',#18238);
#5891=VERTEX_POINT('',#18240);
#5892=VERTEX_POINT('',#18242);
#5893=VERTEX_POINT('',#18244);
#5894=VERTEX_POINT('',#18247);
#5895=VERTEX_POINT('',#18249);
#5896=VERTEX_POINT('',#18251);
#5897=VERTEX_POINT('',#18253);
#5898=VERTEX_POINT('',#18255);
#5899=VERTEX_POINT('',#18257);
#5900=VERTEX_POINT('',#18259);
#5901=VERTEX_POINT('',#18261);
#5902=VERTEX_POINT('',#18263);
#5903=VERTEX_POINT('',#18265);
#5904=VERTEX_POINT('',#18267);
#5905=VERTEX_POINT('',#18303);
#5906=VERTEX_POINT('',#18304);
#5907=VERTEX_POINT('',#18306);
#5908=VERTEX_POINT('',#18308);
#5909=VERTEX_POINT('',#18310);
#5910=VERTEX_POINT('',#18312);
#5911=VERTEX_POINT('',#18314);
#5912=VERTEX_POINT('',#18316);
#5913=VERTEX_POINT('',#18319);
#5914=VERTEX_POINT('',#18321);
#5915=VERTEX_POINT('',#18323);
#5916=VERTEX_POINT('',#18325);
#5917=VERTEX_POINT('',#18327);
#5918=VERTEX_POINT('',#18329);
#5919=VERTEX_POINT('',#18331);
#5920=VERTEX_POINT('',#18333);
#5921=VERTEX_POINT('',#18335);
#5922=VERTEX_POINT('',#18337);
#5923=VERTEX_POINT('',#18339);
#5924=VERTEX_POINT('',#18342);
#5925=VERTEX_POINT('',#18346);
#5926=VERTEX_POINT('',#18350);
#5927=VERTEX_POINT('',#18354);
#5928=VERTEX_POINT('',#18358);
#5929=VERTEX_POINT('',#18362);
#5930=VERTEX_POINT('',#18366);
#5931=VERTEX_POINT('',#18370);
#5932=VERTEX_POINT('',#18374);
#5933=VERTEX_POINT('',#18378);
#5934=VERTEX_POINT('',#18382);
#5935=VERTEX_POINT('',#18386);
#5936=VERTEX_POINT('',#18388);
#5937=VERTEX_POINT('',#18392);
#5938=VERTEX_POINT('',#18394);
#5939=VERTEX_POINT('',#18398);
#5940=VERTEX_POINT('',#18402);
#5941=VERTEX_POINT('',#18408);
#5942=VERTEX_POINT('',#18409);
#5943=VERTEX_POINT('',#18414);
#5944=VERTEX_POINT('',#18416);
#5945=VERTEX_POINT('',#18423);
#5946=VERTEX_POINT('',#18427);
#5947=VERTEX_POINT('',#18435);
#5948=VERTEX_POINT('',#18437);
#5949=VERTEX_POINT('',#18441);
#5950=VERTEX_POINT('',#18442);
#5951=VERTEX_POINT('',#18444);
#5952=VERTEX_POINT('',#18446);
#5953=VERTEX_POINT('',#18450);
#5954=VERTEX_POINT('',#18452);
#5955=VERTEX_POINT('',#18456);
#5956=VERTEX_POINT('',#18458);
#5957=VERTEX_POINT('',#18462);
#5958=VERTEX_POINT('',#18464);
#5959=VERTEX_POINT('',#18468);
#5960=VERTEX_POINT('',#18470);
#5961=VERTEX_POINT('',#18480);
#5962=VERTEX_POINT('',#18482);
#5963=VERTEX_POINT('',#18486);
#5964=VERTEX_POINT('',#18488);
#5965=VERTEX_POINT('',#18492);
#5966=VERTEX_POINT('',#18494);
#5967=VERTEX_POINT('',#18498);
#5968=VERTEX_POINT('',#18499);
#5969=VERTEX_POINT('',#18501);
#5970=VERTEX_POINT('',#18503);
#5971=VERTEX_POINT('',#18507);
#5972=VERTEX_POINT('',#18509);
#5973=VERTEX_POINT('',#18511);
#5974=VERTEX_POINT('',#18513);
#5975=VERTEX_POINT('',#18515);
#5976=VERTEX_POINT('',#18517);
#5977=VERTEX_POINT('',#18520);
#5978=VERTEX_POINT('',#18522);
#5979=VERTEX_POINT('',#18524);
#5980=VERTEX_POINT('',#18526);
#5981=VERTEX_POINT('',#18528);
#5982=VERTEX_POINT('',#18530);
#5983=VERTEX_POINT('',#18532);
#5984=VERTEX_POINT('',#18534);
#5985=VERTEX_POINT('',#18536);
#5986=VERTEX_POINT('',#18538);
#5987=VERTEX_POINT('',#18540);
#5988=VERTEX_POINT('',#18543);
#5989=VERTEX_POINT('',#18544);
#5990=VERTEX_POINT('',#18546);
#5991=VERTEX_POINT('',#18548);
#5992=VERTEX_POINT('',#18552);
#5993=VERTEX_POINT('',#18554);
#5994=VERTEX_POINT('',#18556);
#5995=VERTEX_POINT('',#18558);
#5996=VERTEX_POINT('',#18560);
#5997=VERTEX_POINT('',#18562);
#5998=VERTEX_POINT('',#18565);
#5999=VERTEX_POINT('',#18567);
#6000=VERTEX_POINT('',#18569);
#6001=VERTEX_POINT('',#18571);
#6002=VERTEX_POINT('',#18573);
#6003=VERTEX_POINT('',#18575);
#6004=VERTEX_POINT('',#18577);
#6005=VERTEX_POINT('',#18579);
#6006=VERTEX_POINT('',#18581);
#6007=VERTEX_POINT('',#18583);
#6008=VERTEX_POINT('',#18585);
#6009=VERTEX_POINT('',#18621);
#6010=VERTEX_POINT('',#18622);
#6011=VERTEX_POINT('',#18624);
#6012=VERTEX_POINT('',#18626);
#6013=VERTEX_POINT('',#18628);
#6014=VERTEX_POINT('',#18630);
#6015=VERTEX_POINT('',#18632);
#6016=VERTEX_POINT('',#18634);
#6017=VERTEX_POINT('',#18637);
#6018=VERTEX_POINT('',#18639);
#6019=VERTEX_POINT('',#18641);
#6020=VERTEX_POINT('',#18643);
#6021=VERTEX_POINT('',#18645);
#6022=VERTEX_POINT('',#18647);
#6023=VERTEX_POINT('',#18649);
#6024=VERTEX_POINT('',#18651);
#6025=VERTEX_POINT('',#18653);
#6026=VERTEX_POINT('',#18655);
#6027=VERTEX_POINT('',#18657);
#6028=VERTEX_POINT('',#18660);
#6029=VERTEX_POINT('',#18664);
#6030=VERTEX_POINT('',#18668);
#6031=VERTEX_POINT('',#18672);
#6032=VERTEX_POINT('',#18676);
#6033=VERTEX_POINT('',#18680);
#6034=VERTEX_POINT('',#18684);
#6035=VERTEX_POINT('',#18688);
#6036=VERTEX_POINT('',#18692);
#6037=VERTEX_POINT('',#18696);
#6038=VERTEX_POINT('',#18700);
#6039=VERTEX_POINT('',#18704);
#6040=VERTEX_POINT('',#18706);
#6041=VERTEX_POINT('',#18710);
#6042=VERTEX_POINT('',#18712);
#6043=VERTEX_POINT('',#18716);
#6044=VERTEX_POINT('',#18720);
#6045=VERTEX_POINT('',#18726);
#6046=VERTEX_POINT('',#18727);
#6047=VERTEX_POINT('',#18732);
#6048=VERTEX_POINT('',#18734);
#6049=VERTEX_POINT('',#18741);
#6050=VERTEX_POINT('',#18745);
#6051=VERTEX_POINT('',#18753);
#6052=VERTEX_POINT('',#18754);
#6053=VERTEX_POINT('',#18756);
#6054=VERTEX_POINT('',#18758);
#6055=VERTEX_POINT('',#18760);
#6056=VERTEX_POINT('',#18762);
#6057=VERTEX_POINT('',#18765);
#6058=VERTEX_POINT('',#18768);
#6059=VERTEX_POINT('',#18770);
#6060=VERTEX_POINT('',#18774);
#6061=VERTEX_POINT('',#18778);
#6062=VERTEX_POINT('',#18782);
#6063=VERTEX_POINT('',#18786);
#6064=VERTEX_POINT('',#18793);
#6065=VERTEX_POINT('',#18799);
#6066=VERTEX_POINT('',#18801);
#6067=VERTEX_POINT('',#18805);
#6068=VERTEX_POINT('',#18806);
#6069=VERTEX_POINT('',#18808);
#6070=VERTEX_POINT('',#18810);
#6071=VERTEX_POINT('',#18814);
#6072=VERTEX_POINT('',#18816);
#6073=VERTEX_POINT('',#18820);
#6074=VERTEX_POINT('',#18822);
#6075=VERTEX_POINT('',#18826);
#6076=VERTEX_POINT('',#18828);
#6077=VERTEX_POINT('',#18832);
#6078=VERTEX_POINT('',#18834);
#6079=VERTEX_POINT('',#18844);
#6080=VERTEX_POINT('',#18846);
#6081=VERTEX_POINT('',#18850);
#6082=VERTEX_POINT('',#18851);
#6083=VERTEX_POINT('',#18853);
#6084=VERTEX_POINT('',#18855);
#6085=VERTEX_POINT('',#18859);
#6086=VERTEX_POINT('',#18861);
#6087=VERTEX_POINT('',#18865);
#6088=VERTEX_POINT('',#18867);
#6089=VERTEX_POINT('',#18871);
#6090=VERTEX_POINT('',#18873);
#6091=VERTEX_POINT('',#18877);
#6092=VERTEX_POINT('',#18879);
#6093=VERTEX_POINT('',#18889);
#6094=VERTEX_POINT('',#18890);
#6095=VERTEX_POINT('',#18892);
#6096=VERTEX_POINT('',#18894);
#6097=VERTEX_POINT('',#18898);
#6098=VERTEX_POINT('',#18900);
#6099=VERTEX_POINT('',#18904);
#6100=VERTEX_POINT('',#18906);
#6101=VERTEX_POINT('',#18910);
#6102=VERTEX_POINT('',#18911);
#6103=VERTEX_POINT('',#18913);
#6104=VERTEX_POINT('',#18915);
#6105=VERTEX_POINT('',#18919);
#6106=VERTEX_POINT('',#18921);
#6107=VERTEX_POINT('',#18925);
#6108=VERTEX_POINT('',#18927);
#6109=VERTEX_POINT('',#18931);
#6110=VERTEX_POINT('',#18933);
#6111=VERTEX_POINT('',#18937);
#6112=VERTEX_POINT('',#18939);
#6113=VERTEX_POINT('',#18943);
#6114=VERTEX_POINT('',#18945);
#6115=VERTEX_POINT('',#18949);
#6116=VERTEX_POINT('',#18950);
#6117=VERTEX_POINT('',#18952);
#6118=VERTEX_POINT('',#18954);
#6119=VERTEX_POINT('',#18958);
#6120=VERTEX_POINT('',#18960);
#6121=VERTEX_POINT('',#18964);
#6122=VERTEX_POINT('',#18966);
#6123=VERTEX_POINT('',#18970);
#6124=VERTEX_POINT('',#18971);
#6125=VERTEX_POINT('',#18973);
#6126=VERTEX_POINT('',#18975);
#6127=VERTEX_POINT('',#18979);
#6128=VERTEX_POINT('',#18981);
#6129=VERTEX_POINT('',#18985);
#6130=VERTEX_POINT('',#18987);
#6131=VERTEX_POINT('',#18994);
#6132=VERTEX_POINT('',#18996);
#6133=VERTEX_POINT('',#19003);
#6134=VERTEX_POINT('',#19005);
#6135=VERTEX_POINT('',#19009);
#6136=VERTEX_POINT('',#19011);
#6137=VERTEX_POINT('',#19018);
#6138=VERTEX_POINT('',#19020);
#6139=VERTEX_POINT('',#19024);
#6140=VERTEX_POINT('',#19026);
#6141=VERTEX_POINT('',#19030);
#6142=VERTEX_POINT('',#19032);
#6143=VERTEX_POINT('',#19036);
#6144=VERTEX_POINT('',#19038);
#6145=VERTEX_POINT('',#19042);
#6146=VERTEX_POINT('',#19044);
#6147=VERTEX_POINT('',#19048);
#6148=VERTEX_POINT('',#19050);
#6149=VERTEX_POINT('',#19054);
#6150=VERTEX_POINT('',#19056);
#6151=VERTEX_POINT('',#19060);
#6152=VERTEX_POINT('',#19062);
#6153=VERTEX_POINT('',#19066);
#6154=VERTEX_POINT('',#19068);
#6155=VERTEX_POINT('',#19072);
#6156=VERTEX_POINT('',#19074);
#6157=VERTEX_POINT('',#19078);
#6158=VERTEX_POINT('',#19080);
#6159=VERTEX_POINT('',#19084);
#6160=VERTEX_POINT('',#19086);
#6161=VERTEX_POINT('',#19090);
#6162=VERTEX_POINT('',#19092);
#6163=VERTEX_POINT('',#19096);
#6164=VERTEX_POINT('',#19098);
#6165=VERTEX_POINT('',#19102);
#6166=VERTEX_POINT('',#19104);
#6167=VERTEX_POINT('',#19108);
#6168=VERTEX_POINT('',#19110);
#6169=VERTEX_POINT('',#19114);
#6170=VERTEX_POINT('',#19116);
#6171=VERTEX_POINT('',#19120);
#6172=VERTEX_POINT('',#19122);
#6173=VERTEX_POINT('',#19132);
#6174=VERTEX_POINT('',#19134);
#6175=VERTEX_POINT('',#19138);
#6176=VERTEX_POINT('',#19139);
#6177=VERTEX_POINT('',#19141);
#6178=VERTEX_POINT('',#19143);
#6179=VERTEX_POINT('',#19147);
#6180=VERTEX_POINT('',#19149);
#6181=VERTEX_POINT('',#19153);
#6182=VERTEX_POINT('',#19155);
#6183=VERTEX_POINT('',#19159);
#6184=VERTEX_POINT('',#19161);
#6185=VERTEX_POINT('',#19165);
#6186=VERTEX_POINT('',#19167);
#6187=EDGE_CURVE('',#5171,#5171,#4501,.T.);
#6188=EDGE_CURVE('',#5171,#5172,#4502,.T.);
#6189=EDGE_CURVE('',#5172,#5173,#4503,.T.);
#6190=EDGE_CURVE('',#5173,#5172,#4504,.T.);
#6191=EDGE_CURVE('',#5173,#5174,#839,.T.);
#6192=EDGE_CURVE('',#5175,#5174,#4505,.T.);
#6193=EDGE_CURVE('',#5174,#5175,#4506,.T.);
#6194=EDGE_CURVE('',#5175,#5176,#4507,.T.);
#6195=EDGE_CURVE('',#5176,#5176,#4508,.T.);
#6196=EDGE_CURVE('',#5177,#5178,#4509,.T.);
#6197=EDGE_CURVE('',#5178,#5179,#4510,.T.);
#6198=EDGE_CURVE('',#5179,#5179,#4511,.T.);
#6199=EDGE_CURVE('',#5178,#5177,#4512,.T.);
#6200=EDGE_CURVE('',#5180,#5181,#4513,.T.);
#6201=EDGE_CURVE('',#5180,#5177,#840,.T.);
#6202=EDGE_CURVE('',#5181,#5180,#4514,.T.);
#6203=EDGE_CURVE('',#5176,#5181,#4515,.T.);
#6204=EDGE_CURVE('',#5182,#5182,#4516,.T.);
#6205=EDGE_CURVE('',#5182,#5183,#841,.T.);
#6206=EDGE_CURVE('',#5183,#5183,#4517,.T.);
#6207=EDGE_CURVE('',#5184,#5184,#4518,.T.);
#6208=EDGE_CURVE('',#5184,#5185,#4519,.T.);
#6209=EDGE_CURVE('',#5185,#5186,#4520,.T.);
#6210=EDGE_CURVE('',#5186,#5185,#4521,.T.);
#6211=EDGE_CURVE('',#5186,#5187,#842,.T.);
#6212=EDGE_CURVE('',#5188,#5187,#4522,.T.);
#6213=EDGE_CURVE('',#5187,#5188,#4523,.T.);
#6214=EDGE_CURVE('',#5179,#5188,#4524,.T.);
#6215=EDGE_CURVE('',#5189,#5189,#4525,.T.);
#6216=EDGE_CURVE('',#5190,#5190,#4526,.T.);
#6217=EDGE_CURVE('',#5189,#5191,#843,.T.);
#6218=EDGE_CURVE('',#5191,#5191,#4527,.T.);
#6219=EDGE_CURVE('',#5192,#5192,#4528,.T.);
#6220=EDGE_CURVE('',#5193,#5193,#4529,.T.);
#6221=EDGE_CURVE('',#5194,#5194,#4530,.T.);
#6222=EDGE_CURVE('',#5195,#5195,#4531,.T.);
#6223=EDGE_CURVE('',#5196,#5196,#4532,.T.);
#6224=EDGE_CURVE('',#5193,#5195,#844,.T.);
#6225=EDGE_CURVE('',#5190,#5196,#845,.T.);
#6226=EDGE_CURVE('',#5197,#5197,#4533,.T.);
#6227=EDGE_CURVE('',#5198,#5198,#4534,.T.);
#6228=EDGE_CURVE('',#5199,#5199,#4535,.T.);
#6229=EDGE_CURVE('',#5199,#5197,#846,.T.);
#6230=EDGE_CURVE('',#5200,#5200,#4536,.T.);
#6231=EDGE_CURVE('',#5192,#5201,#847,.T.);
#6232=EDGE_CURVE('',#5201,#5201,#4537,.T.);
#6233=EDGE_CURVE('',#5202,#5202,#4538,.T.);
#6234=EDGE_CURVE('',#5202,#5200,#848,.T.);
#6235=EDGE_CURVE('',#5194,#5198,#849,.T.);
#6236=EDGE_CURVE('',#5203,#5203,#4539,.T.);
#6237=EDGE_CURVE('',#5204,#5204,#4540,.T.);
#6238=EDGE_CURVE('',#5204,#5203,#850,.T.);
#6239=EDGE_CURVE('',#5205,#5206,#4541,.T.);
#6240=EDGE_CURVE('',#5206,#5207,#851,.T.);
#6241=EDGE_CURVE('',#5207,#5208,#4542,.T.);
#6242=EDGE_CURVE('',#5208,#5205,#852,.T.);
#6243=EDGE_CURVE('',#5209,#5208,#853,.T.);
#6244=EDGE_CURVE('',#5210,#5209,#854,.T.);
#6245=EDGE_CURVE('',#5205,#5210,#855,.T.);
#6246=EDGE_CURVE('',#5211,#5211,#4543,.T.);
#6247=EDGE_CURVE('',#5212,#5212,#4544,.T.);
#6248=EDGE_CURVE('',#5213,#5213,#4545,.T.);
#6249=EDGE_CURVE('',#5214,#5214,#4546,.T.);
#6250=EDGE_CURVE('',#5215,#5215,#4547,.T.);
#6251=EDGE_CURVE('',#5216,#5216,#4548,.T.);
#6252=EDGE_CURVE('',#5217,#5217,#4549,.T.);
#6253=EDGE_CURVE('',#5218,#5218,#4550,.T.);
#6254=EDGE_CURVE('',#5219,#5219,#4551,.T.);
#6255=EDGE_CURVE('',#5220,#5220,#4552,.T.);
#6256=EDGE_CURVE('',#5221,#5221,#4553,.T.);
#6257=EDGE_CURVE('',#5207,#5222,#856,.T.);
#6258=EDGE_CURVE('',#5222,#5223,#857,.T.);
#6259=EDGE_CURVE('',#5224,#5223,#858,.T.);
#6260=EDGE_CURVE('',#5225,#5224,#859,.T.);
#6261=EDGE_CURVE('',#5226,#5225,#860,.T.);
#6262=EDGE_CURVE('',#5226,#5227,#861,.T.);
#6263=EDGE_CURVE('',#5227,#5228,#862,.T.);
#6264=EDGE_CURVE('',#5209,#5228,#4554,.T.);
#6265=EDGE_CURVE('',#5229,#5210,#4555,.T.);
#6266=EDGE_CURVE('',#5228,#5229,#863,.T.);
#6267=EDGE_CURVE('',#5230,#5230,#4556,.T.);
#6268=EDGE_CURVE('',#5230,#5231,#864,.T.);
#6269=EDGE_CURVE('',#5231,#5231,#4557,.T.);
#6270=EDGE_CURVE('',#5232,#5232,#4558,.T.);
#6271=EDGE_CURVE('',#5232,#5233,#865,.T.);
#6272=EDGE_CURVE('',#5233,#5233,#4559,.T.);
#6273=EDGE_CURVE('',#5234,#5234,#4560,.T.);
#6274=EDGE_CURVE('',#5234,#5235,#866,.T.);
#6275=EDGE_CURVE('',#5235,#5235,#4561,.T.);
#6276=EDGE_CURVE('',#5236,#5236,#4562,.T.);
#6277=EDGE_CURVE('',#5236,#5237,#867,.T.);
#6278=EDGE_CURVE('',#5237,#5237,#4563,.T.);
#6279=EDGE_CURVE('',#5238,#5238,#4564,.T.);
#6280=EDGE_CURVE('',#5238,#5239,#868,.T.);
#6281=EDGE_CURVE('',#5239,#5239,#4565,.T.);
#6282=EDGE_CURVE('',#5240,#5240,#4566,.T.);
#6283=EDGE_CURVE('',#5240,#5241,#869,.T.);
#6284=EDGE_CURVE('',#5241,#5241,#4567,.T.);
#6285=EDGE_CURVE('',#5242,#5242,#4568,.T.);
#6286=EDGE_CURVE('',#5242,#5243,#870,.T.);
#6287=EDGE_CURVE('',#5243,#5243,#4569,.T.);
#6288=EDGE_CURVE('',#5244,#5244,#4570,.T.);
#6289=EDGE_CURVE('',#5244,#5245,#871,.T.);
#6290=EDGE_CURVE('',#5245,#5245,#4571,.T.);
#6291=EDGE_CURVE('',#5246,#5246,#4572,.T.);
#6292=EDGE_CURVE('',#5246,#5247,#872,.T.);
#6293=EDGE_CURVE('',#5247,#5247,#4573,.T.);
#6294=EDGE_CURVE('',#5248,#5248,#4574,.T.);
#6295=EDGE_CURVE('',#5248,#5249,#873,.T.);
#6296=EDGE_CURVE('',#5249,#5249,#4575,.T.);
#6297=EDGE_CURVE('',#5250,#5250,#4576,.T.);
#6298=EDGE_CURVE('',#5250,#5251,#874,.T.);
#6299=EDGE_CURVE('',#5251,#5251,#4577,.T.);
#6300=EDGE_CURVE('',#5221,#5252,#875,.T.);
#6301=EDGE_CURVE('',#5252,#5252,#4578,.T.);
#6302=EDGE_CURVE('',#5220,#5253,#876,.T.);
#6303=EDGE_CURVE('',#5253,#5253,#4579,.T.);
#6304=EDGE_CURVE('',#5219,#5254,#877,.T.);
#6305=EDGE_CURVE('',#5254,#5254,#4580,.T.);
#6306=EDGE_CURVE('',#5218,#5255,#878,.T.);
#6307=EDGE_CURVE('',#5255,#5255,#4581,.T.);
#6308=EDGE_CURVE('',#5217,#5256,#879,.T.);
#6309=EDGE_CURVE('',#5256,#5256,#4582,.T.);
#6310=EDGE_CURVE('',#5216,#5257,#880,.T.);
#6311=EDGE_CURVE('',#5257,#5257,#4583,.T.);
#6312=EDGE_CURVE('',#5215,#5258,#881,.T.);
#6313=EDGE_CURVE('',#5258,#5258,#4584,.T.);
#6314=EDGE_CURVE('',#5214,#5259,#882,.T.);
#6315=EDGE_CURVE('',#5259,#5259,#4585,.T.);
#6316=EDGE_CURVE('',#5213,#5260,#883,.T.);
#6317=EDGE_CURVE('',#5260,#5260,#4586,.T.);
#6318=EDGE_CURVE('',#5212,#5261,#884,.T.);
#6319=EDGE_CURVE('',#5261,#5261,#4587,.T.);
#6320=EDGE_CURVE('',#5211,#5262,#885,.T.);
#6321=EDGE_CURVE('',#5262,#5262,#4588,.T.);
#6322=EDGE_CURVE('',#5263,#5263,#4589,.T.);
#6323=EDGE_CURVE('',#5263,#5264,#886,.T.);
#6324=EDGE_CURVE('',#5264,#5264,#4590,.T.);
#6325=EDGE_CURVE('',#5265,#5265,#4591,.T.);
#6326=EDGE_CURVE('',#5265,#5266,#887,.T.);
#6327=EDGE_CURVE('',#5266,#5266,#4592,.T.);
#6328=EDGE_CURVE('',#5267,#5267,#4593,.T.);
#6329=EDGE_CURVE('',#5267,#5268,#888,.T.);
#6330=EDGE_CURVE('',#5268,#5268,#4594,.T.);
#6331=EDGE_CURVE('',#5269,#5269,#4595,.T.);
#6332=EDGE_CURVE('',#5269,#5270,#889,.T.);
#6333=EDGE_CURVE('',#5270,#5270,#4596,.T.);
#6334=EDGE_CURVE('',#5271,#5271,#4597,.T.);
#6335=EDGE_CURVE('',#5271,#5272,#890,.T.);
#6336=EDGE_CURVE('',#5272,#5272,#4598,.T.);
#6337=EDGE_CURVE('',#5273,#5273,#4599,.T.);
#6338=EDGE_CURVE('',#5273,#5274,#891,.T.);
#6339=EDGE_CURVE('',#5274,#5274,#4600,.T.);
#6340=EDGE_CURVE('',#5275,#5275,#4601,.T.);
#6341=EDGE_CURVE('',#5275,#5276,#892,.T.);
#6342=EDGE_CURVE('',#5276,#5276,#4602,.T.);
#6343=EDGE_CURVE('',#5277,#5277,#4603,.T.);
#6344=EDGE_CURVE('',#5277,#5278,#893,.T.);
#6345=EDGE_CURVE('',#5278,#5278,#4604,.T.);
#6346=EDGE_CURVE('',#5279,#5279,#4605,.T.);
#6347=EDGE_CURVE('',#5279,#5280,#894,.T.);
#6348=EDGE_CURVE('',#5280,#5280,#4606,.T.);
#6349=EDGE_CURVE('',#5281,#5281,#4607,.T.);
#6350=EDGE_CURVE('',#5281,#5282,#895,.T.);
#6351=EDGE_CURVE('',#5282,#5282,#4608,.T.);
#6352=EDGE_CURVE('',#5283,#5283,#4609,.T.);
#6353=EDGE_CURVE('',#5283,#5284,#896,.T.);
#6354=EDGE_CURVE('',#5284,#5284,#4610,.T.);
#6355=EDGE_CURVE('',#5226,#5285,#897,.T.);
#6356=EDGE_CURVE('',#5286,#5285,#898,.T.);
#6357=EDGE_CURVE('',#5227,#5286,#899,.T.);
#6358=EDGE_CURVE('',#5229,#5286,#900,.T.);
#6359=EDGE_CURVE('',#5287,#5206,#901,.T.);
#6360=EDGE_CURVE('',#5222,#5287,#902,.T.);
#6361=EDGE_CURVE('',#5288,#5287,#903,.T.);
#6362=EDGE_CURVE('',#5223,#5288,#904,.T.);
#6363=EDGE_CURVE('',#5289,#5288,#905,.T.);
#6364=EDGE_CURVE('',#5224,#5289,#906,.T.);
#6365=EDGE_CURVE('',#5290,#5289,#907,.T.);
#6366=EDGE_CURVE('',#5225,#5290,#908,.T.);
#6367=EDGE_CURVE('',#5285,#5290,#909,.T.);
#6368=EDGE_CURVE('',#5291,#5292,#910,.T.);
#6369=EDGE_CURVE('',#5293,#5291,#911,.T.);
#6370=EDGE_CURVE('',#5294,#5293,#912,.T.);
#6371=EDGE_CURVE('',#5295,#5294,#913,.T.);
#6372=EDGE_CURVE('',#5296,#5295,#914,.T.);
#6373=EDGE_CURVE('',#5292,#5296,#915,.T.);
#6374=EDGE_CURVE('',#5297,#5297,#4611,.F.);
#6375=EDGE_CURVE('',#5291,#5298,#916,.T.);
#6376=EDGE_CURVE('',#5299,#5298,#917,.T.);
#6377=EDGE_CURVE('',#5293,#5299,#918,.T.);
#6378=EDGE_CURVE('',#5300,#5299,#919,.T.);
#6379=EDGE_CURVE('',#5294,#5300,#920,.T.);
#6380=EDGE_CURVE('',#5301,#5300,#921,.T.);
#6381=EDGE_CURVE('',#5295,#5301,#922,.T.);
#6382=EDGE_CURVE('',#5302,#5301,#923,.T.);
#6383=EDGE_CURVE('',#5296,#5302,#924,.T.);
#6384=EDGE_CURVE('',#5303,#5302,#925,.T.);
#6385=EDGE_CURVE('',#5292,#5303,#926,.T.);
#6386=EDGE_CURVE('',#5298,#5303,#927,.T.);
#6387=EDGE_CURVE('',#5304,#5304,#4612,.T.);
#6388=EDGE_CURVE('',#5304,#5297,#928,.T.);
#6389=EDGE_CURVE('',#5305,#5306,#929,.T.);
#6390=EDGE_CURVE('',#5306,#5307,#930,.T.);
#6391=EDGE_CURVE('',#5307,#5308,#931,.T.);
#6392=EDGE_CURVE('',#5305,#5308,#932,.T.);
#6393=EDGE_CURVE('',#5309,#5306,#4613,.T.);
#6394=EDGE_CURVE('',#5309,#5310,#933,.T.);
#6395=EDGE_CURVE('',#5310,#5307,#4614,.T.);
#6396=EDGE_CURVE('',#5309,#5311,#934,.T.);
#6397=EDGE_CURVE('',#5312,#5311,#935,.T.);
#6398=EDGE_CURVE('',#5312,#5310,#936,.T.);
#6399=EDGE_CURVE('',#5313,#5314,#937,.T.);
#6400=EDGE_CURVE('',#5313,#5315,#938,.T.);
#6401=EDGE_CURVE('',#5315,#5316,#939,.T.);
#6402=EDGE_CURVE('',#5314,#5316,#940,.T.);
#6403=EDGE_CURVE('',#5313,#5317,#4615,.T.);
#6404=EDGE_CURVE('',#5317,#5318,#941,.T.);
#6405=EDGE_CURVE('',#5318,#5315,#4616,.T.);
#6406=EDGE_CURVE('',#5319,#5317,#942,.T.);
#6407=EDGE_CURVE('',#5319,#5320,#943,.T.);
#6408=EDGE_CURVE('',#5320,#5318,#944,.T.);
#6409=EDGE_CURVE('',#5321,#5319,#4617,.T.);
#6410=EDGE_CURVE('',#5321,#5322,#945,.T.);
#6411=EDGE_CURVE('',#5322,#5320,#4618,.T.);
#6412=EDGE_CURVE('',#5323,#5305,#4619,.T.);
#6413=EDGE_CURVE('',#5308,#5324,#4620,.T.);
#6414=EDGE_CURVE('',#5323,#5324,#946,.T.);
#6415=EDGE_CURVE('',#5321,#5325,#947,.T.);
#6416=EDGE_CURVE('',#5325,#5326,#948,.T.);
#6417=EDGE_CURVE('',#5326,#5322,#949,.T.);
#6418=EDGE_CURVE('',#5327,#5328,#950,.T.);
#6419=EDGE_CURVE('',#5327,#5329,#951,.T.);
#6420=EDGE_CURVE('',#5330,#5329,#952,.T.);
#6421=EDGE_CURVE('',#5328,#5330,#953,.T.);
#6422=EDGE_CURVE('',#5331,#5328,#4621,.T.);
#6423=EDGE_CURVE('',#5332,#5330,#4622,.T.);
#6424=EDGE_CURVE('',#5331,#5332,#954,.T.);
#6425=EDGE_CURVE('',#5331,#5333,#955,.T.);
#6426=EDGE_CURVE('',#5334,#5332,#956,.T.);
#6427=EDGE_CURVE('',#5333,#5334,#957,.T.);
#6428=EDGE_CURVE('',#5335,#5336,#958,.T.);
#6429=EDGE_CURVE('',#5337,#5336,#959,.T.);
#6430=EDGE_CURVE('',#5338,#5337,#960,.T.);
#6431=EDGE_CURVE('',#5335,#5338,#961,.T.);
#6432=EDGE_CURVE('',#5335,#5339,#4623,.T.);
#6433=EDGE_CURVE('',#5340,#5338,#4624,.T.);
#6434=EDGE_CURVE('',#5339,#5340,#962,.T.);
#6435=EDGE_CURVE('',#5341,#5339,#963,.T.);
#6436=EDGE_CURVE('',#5342,#5340,#964,.T.);
#6437=EDGE_CURVE('',#5341,#5342,#965,.T.);
#6438=EDGE_CURVE('',#5325,#5341,#4625,.T.);
#6439=EDGE_CURVE('',#5326,#5342,#4626,.T.);
#6440=EDGE_CURVE('',#5343,#5324,#966,.T.);
#6441=EDGE_CURVE('',#5344,#5343,#967,.T.);
#6442=EDGE_CURVE('',#5323,#5344,#968,.T.);
#6443=EDGE_CURVE('',#5344,#5327,#4627,.T.);
#6444=EDGE_CURVE('',#5329,#5343,#4628,.T.);
#6445=EDGE_CURVE('',#5345,#5334,#969,.T.);
#6446=EDGE_CURVE('',#5346,#5345,#970,.T.);
#6447=EDGE_CURVE('',#5346,#5333,#971,.T.);
#6448=EDGE_CURVE('',#5311,#5347,#972,.T.);
#6449=EDGE_CURVE('',#5347,#5348,#973,.T.);
#6450=EDGE_CURVE('',#5312,#5348,#974,.T.);
#6451=EDGE_CURVE('',#5337,#5316,#975,.T.);
#6452=EDGE_CURVE('',#5336,#5314,#976,.T.);
#6453=EDGE_CURVE('',#5349,#5347,#4629,.T.);
#6454=EDGE_CURVE('',#5349,#5350,#977,.T.);
#6455=EDGE_CURVE('',#5350,#5348,#4630,.T.);
#6456=EDGE_CURVE('',#5349,#5351,#978,.T.);
#6457=EDGE_CURVE('',#5351,#5352,#979,.T.);
#6458=EDGE_CURVE('',#5352,#5350,#980,.T.);
#6459=EDGE_CURVE('',#5353,#5351,#4631,.T.);
#6460=EDGE_CURVE('',#5353,#5354,#981,.T.);
#6461=EDGE_CURVE('',#5354,#5352,#4632,.T.);
#6462=EDGE_CURVE('',#5353,#5355,#982,.T.);
#6463=EDGE_CURVE('',#5355,#5356,#983,.T.);
#6464=EDGE_CURVE('',#5356,#5354,#984,.T.);
#6465=EDGE_CURVE('',#5357,#5355,#985,.T.);
#6466=EDGE_CURVE('',#5357,#5358,#986,.T.);
#6467=EDGE_CURVE('',#5358,#5356,#987,.T.);
#6468=EDGE_CURVE('',#5359,#5357,#988,.T.);
#6469=EDGE_CURVE('',#5359,#5360,#989,.T.);
#6470=EDGE_CURVE('',#5360,#5358,#990,.T.);
#6471=EDGE_CURVE('',#5359,#5361,#4633,.T.);
#6472=EDGE_CURVE('',#5361,#5362,#991,.T.);
#6473=EDGE_CURVE('',#5362,#5360,#4634,.T.);
#6474=EDGE_CURVE('',#5363,#5361,#992,.T.);
#6475=EDGE_CURVE('',#5363,#5364,#993,.T.);
#6476=EDGE_CURVE('',#5364,#5362,#994,.T.);
#6477=EDGE_CURVE('',#5363,#5365,#4635,.T.);
#6478=EDGE_CURVE('',#5365,#5366,#995,.T.);
#6479=EDGE_CURVE('',#5366,#5364,#4636,.T.);
#6480=EDGE_CURVE('',#5365,#5367,#996,.T.);
#6481=EDGE_CURVE('',#5367,#5368,#997,.T.);
#6482=EDGE_CURVE('',#5368,#5366,#998,.T.);
#6483=EDGE_CURVE('',#5369,#5346,#4637,.T.);
#6484=EDGE_CURVE('',#5370,#5345,#4638,.T.);
#6485=EDGE_CURVE('',#5369,#5370,#999,.T.);
#6486=EDGE_CURVE('',#5369,#5371,#1000,.T.);
#6487=EDGE_CURVE('',#5372,#5370,#1001,.T.);
#6488=EDGE_CURVE('',#5371,#5372,#1002,.T.);
#6489=EDGE_CURVE('',#5373,#5371,#4639,.T.);
#6490=EDGE_CURVE('',#5374,#5372,#4640,.T.);
#6491=EDGE_CURVE('',#5373,#5374,#1003,.T.);
#6492=EDGE_CURVE('',#5373,#5375,#1004,.T.);
#6493=EDGE_CURVE('',#5376,#5374,#1005,.T.);
#6494=EDGE_CURVE('',#5375,#5376,#1006,.T.);
#6495=EDGE_CURVE('',#5377,#5375,#1007,.T.);
#6496=EDGE_CURVE('',#5378,#5376,#1008,.T.);
#6497=EDGE_CURVE('',#5377,#5378,#1009,.T.);
#6498=EDGE_CURVE('',#5379,#5377,#1010,.T.);
#6499=EDGE_CURVE('',#5380,#5378,#1011,.T.);
#6500=EDGE_CURVE('',#5379,#5380,#1012,.T.);
#6501=EDGE_CURVE('',#5379,#5381,#4641,.T.);
#6502=EDGE_CURVE('',#5382,#5380,#4642,.T.);
#6503=EDGE_CURVE('',#5381,#5382,#1013,.T.);
#6504=EDGE_CURVE('',#5383,#5381,#1014,.T.);
#6505=EDGE_CURVE('',#5384,#5382,#1015,.T.);
#6506=EDGE_CURVE('',#5383,#5384,#1016,.T.);
#6507=EDGE_CURVE('',#5383,#5367,#4643,.T.);
#6508=EDGE_CURVE('',#5368,#5384,#4644,.T.);
#6509=EDGE_CURVE('',#5385,#5385,#4645,.T.);
#6510=EDGE_CURVE('',#5385,#5386,#1017,.T.);
#6511=EDGE_CURVE('',#5386,#5386,#4646,.T.);
#6512=EDGE_CURVE('',#5387,#5387,#4647,.T.);
#6513=EDGE_CURVE('',#5387,#5388,#1018,.T.);
#6514=EDGE_CURVE('',#5388,#5388,#4648,.T.);
#6515=EDGE_CURVE('',#5389,#5389,#4649,.T.);
#6516=EDGE_CURVE('',#5389,#5390,#1019,.T.);
#6517=EDGE_CURVE('',#5390,#5390,#4650,.T.);
#6518=EDGE_CURVE('',#5391,#5391,#4651,.T.);
#6519=EDGE_CURVE('',#5391,#5392,#1020,.T.);
#6520=EDGE_CURVE('',#5392,#5392,#4652,.T.);
#6521=EDGE_CURVE('',#5393,#5393,#4653,.T.);
#6522=EDGE_CURVE('',#5393,#5394,#1021,.T.);
#6523=EDGE_CURVE('',#5394,#5394,#4654,.T.);
#6524=EDGE_CURVE('',#5395,#5396,#1022,.T.);
#6525=EDGE_CURVE('',#5397,#5395,#1023,.T.);
#6526=EDGE_CURVE('',#5398,#5397,#1024,.T.);
#6527=EDGE_CURVE('',#5398,#5396,#1025,.T.);
#6528=EDGE_CURVE('',#5396,#5399,#4655,.T.);
#6529=EDGE_CURVE('',#5400,#5398,#4656,.T.);
#6530=EDGE_CURVE('',#5400,#5399,#1026,.T.);
#6531=EDGE_CURVE('',#5399,#5401,#1027,.T.);
#6532=EDGE_CURVE('',#5402,#5400,#1028,.T.);
#6533=EDGE_CURVE('',#5402,#5401,#1029,.T.);
#6534=EDGE_CURVE('',#5401,#5395,#4657,.T.);
#6535=EDGE_CURVE('',#5397,#5402,#4658,.T.);
#6536=EDGE_CURVE('',#5403,#5404,#1030,.T.);
#6537=EDGE_CURVE('',#5405,#5403,#1031,.T.);
#6538=EDGE_CURVE('',#5406,#5405,#1032,.T.);
#6539=EDGE_CURVE('',#5406,#5404,#1033,.T.);
#6540=EDGE_CURVE('',#5404,#5407,#4659,.T.);
#6541=EDGE_CURVE('',#5408,#5406,#4660,.T.);
#6542=EDGE_CURVE('',#5408,#5407,#1034,.T.);
#6543=EDGE_CURVE('',#5407,#5409,#1035,.T.);
#6544=EDGE_CURVE('',#5410,#5408,#1036,.T.);
#6545=EDGE_CURVE('',#5410,#5409,#1037,.T.);
#6546=EDGE_CURVE('',#5409,#5403,#4661,.T.);
#6547=EDGE_CURVE('',#5405,#5410,#4662,.T.);
#6548=EDGE_CURVE('',#5411,#5411,#4663,.T.);
#6549=EDGE_CURVE('',#5411,#5412,#1038,.T.);
#6550=EDGE_CURVE('',#5412,#5412,#4664,.T.);
#6551=EDGE_CURVE('',#5413,#5413,#4665,.T.);
#6552=EDGE_CURVE('',#5413,#5414,#1039,.T.);
#6553=EDGE_CURVE('',#5414,#5414,#4666,.T.);
#6554=EDGE_CURVE('',#5415,#5415,#4667,.T.);
#6555=EDGE_CURVE('',#5415,#5416,#1040,.T.);
#6556=EDGE_CURVE('',#5416,#5416,#4668,.T.);
#6557=EDGE_CURVE('',#5417,#5417,#4669,.T.);
#6558=EDGE_CURVE('',#5417,#5418,#1041,.T.);
#6559=EDGE_CURVE('',#5418,#5418,#4670,.T.);
#6560=EDGE_CURVE('',#5419,#5419,#4671,.T.);
#6561=EDGE_CURVE('',#5419,#5420,#1042,.T.);
#6562=EDGE_CURVE('',#5420,#5420,#4672,.T.);
#6563=EDGE_CURVE('',#5421,#5422,#1043,.T.);
#6564=EDGE_CURVE('',#5423,#5421,#1044,.T.);
#6565=EDGE_CURVE('',#5424,#5423,#1045,.T.);
#6566=EDGE_CURVE('',#5424,#5422,#1046,.T.);
#6567=EDGE_CURVE('',#5422,#5425,#4673,.T.);
#6568=EDGE_CURVE('',#5426,#5424,#4674,.T.);
#6569=EDGE_CURVE('',#5426,#5425,#1047,.T.);
#6570=EDGE_CURVE('',#5425,#5427,#1048,.T.);
#6571=EDGE_CURVE('',#5428,#5426,#1049,.T.);
#6572=EDGE_CURVE('',#5428,#5427,#1050,.T.);
#6573=EDGE_CURVE('',#5427,#5421,#4675,.T.);
#6574=EDGE_CURVE('',#5423,#5428,#4676,.T.);
#6575=EDGE_CURVE('',#5429,#5430,#1051,.T.);
#6576=EDGE_CURVE('',#5431,#5429,#1052,.T.);
#6577=EDGE_CURVE('',#5432,#5431,#1053,.T.);
#6578=EDGE_CURVE('',#5432,#5430,#1054,.T.);
#6579=EDGE_CURVE('',#5430,#5433,#4677,.T.);
#6580=EDGE_CURVE('',#5434,#5432,#4678,.T.);
#6581=EDGE_CURVE('',#5434,#5433,#1055,.T.);
#6582=EDGE_CURVE('',#5433,#5435,#1056,.T.);
#6583=EDGE_CURVE('',#5436,#5434,#1057,.T.);
#6584=EDGE_CURVE('',#5436,#5435,#1058,.T.);
#6585=EDGE_CURVE('',#5435,#5429,#4679,.T.);
#6586=EDGE_CURVE('',#5431,#5436,#4680,.T.);
#6587=EDGE_CURVE('',#5437,#5437,#4681,.T.);
#6588=EDGE_CURVE('',#5437,#5438,#1059,.T.);
#6589=EDGE_CURVE('',#5438,#5438,#4682,.T.);
#6590=EDGE_CURVE('',#5439,#5439,#4683,.T.);
#6591=EDGE_CURVE('',#5439,#5440,#1060,.T.);
#6592=EDGE_CURVE('',#5440,#5440,#4684,.T.);
#6593=EDGE_CURVE('',#5441,#5441,#4685,.T.);
#6594=EDGE_CURVE('',#5441,#5442,#1061,.T.);
#6595=EDGE_CURVE('',#5442,#5442,#4686,.T.);
#6596=EDGE_CURVE('',#5443,#5443,#4687,.T.);
#6597=EDGE_CURVE('',#5443,#5444,#1062,.T.);
#6598=EDGE_CURVE('',#5444,#5444,#4688,.T.);
#6599=EDGE_CURVE('',#5445,#5445,#4689,.T.);
#6600=EDGE_CURVE('',#5445,#5446,#1063,.T.);
#6601=EDGE_CURVE('',#5446,#5446,#4690,.T.);
#6602=EDGE_CURVE('',#5447,#5448,#1064,.T.);
#6603=EDGE_CURVE('',#5449,#5447,#1065,.T.);
#6604=EDGE_CURVE('',#5450,#5449,#1066,.T.);
#6605=EDGE_CURVE('',#5450,#5448,#1067,.T.);
#6606=EDGE_CURVE('',#5448,#5451,#4691,.T.);
#6607=EDGE_CURVE('',#5452,#5450,#4692,.T.);
#6608=EDGE_CURVE('',#5452,#5451,#1068,.T.);
#6609=EDGE_CURVE('',#5451,#5453,#1069,.T.);
#6610=EDGE_CURVE('',#5454,#5452,#1070,.T.);
#6611=EDGE_CURVE('',#5454,#5453,#1071,.T.);
#6612=EDGE_CURVE('',#5453,#5447,#4693,.T.);
#6613=EDGE_CURVE('',#5449,#5454,#4694,.T.);
#6614=EDGE_CURVE('',#5455,#5456,#1072,.T.);
#6615=EDGE_CURVE('',#5457,#5455,#1073,.T.);
#6616=EDGE_CURVE('',#5458,#5457,#1074,.T.);
#6617=EDGE_CURVE('',#5458,#5456,#1075,.T.);
#6618=EDGE_CURVE('',#5456,#5459,#4695,.T.);
#6619=EDGE_CURVE('',#5460,#5458,#4696,.T.);
#6620=EDGE_CURVE('',#5460,#5459,#1076,.T.);
#6621=EDGE_CURVE('',#5459,#5461,#1077,.T.);
#6622=EDGE_CURVE('',#5462,#5460,#1078,.T.);
#6623=EDGE_CURVE('',#5462,#5461,#1079,.T.);
#6624=EDGE_CURVE('',#5461,#5455,#4697,.T.);
#6625=EDGE_CURVE('',#5457,#5462,#4698,.T.);
#6626=EDGE_CURVE('',#5463,#5463,#4699,.T.);
#6627=EDGE_CURVE('',#5463,#5464,#1080,.T.);
#6628=EDGE_CURVE('',#5464,#5464,#4700,.T.);
#6629=EDGE_CURVE('',#5465,#5465,#4701,.T.);
#6630=EDGE_CURVE('',#5465,#5466,#1081,.T.);
#6631=EDGE_CURVE('',#5466,#5466,#4702,.T.);
#6632=EDGE_CURVE('',#5467,#5467,#4703,.T.);
#6633=EDGE_CURVE('',#5467,#5468,#1082,.T.);
#6634=EDGE_CURVE('',#5468,#5468,#4704,.T.);
#6635=EDGE_CURVE('',#5469,#5469,#4705,.T.);
#6636=EDGE_CURVE('',#5469,#5470,#1083,.T.);
#6637=EDGE_CURVE('',#5470,#5470,#4706,.T.);
#6638=EDGE_CURVE('',#5471,#5471,#4707,.T.);
#6639=EDGE_CURVE('',#5471,#5472,#1084,.T.);
#6640=EDGE_CURVE('',#5472,#5472,#4708,.T.);
#6641=EDGE_CURVE('',#5473,#5474,#1085,.T.);
#6642=EDGE_CURVE('',#5475,#5473,#1086,.T.);
#6643=EDGE_CURVE('',#5476,#5475,#1087,.T.);
#6644=EDGE_CURVE('',#5476,#5474,#1088,.T.);
#6645=EDGE_CURVE('',#5474,#5477,#4709,.T.);
#6646=EDGE_CURVE('',#5478,#5476,#4710,.T.);
#6647=EDGE_CURVE('',#5478,#5477,#1089,.T.);
#6648=EDGE_CURVE('',#5477,#5479,#1090,.T.);
#6649=EDGE_CURVE('',#5480,#5478,#1091,.T.);
#6650=EDGE_CURVE('',#5480,#5479,#1092,.T.);
#6651=EDGE_CURVE('',#5479,#5473,#4711,.T.);
#6652=EDGE_CURVE('',#5475,#5480,#4712,.T.);
#6653=EDGE_CURVE('',#5481,#5482,#1093,.T.);
#6654=EDGE_CURVE('',#5483,#5481,#1094,.T.);
#6655=EDGE_CURVE('',#5484,#5483,#1095,.T.);
#6656=EDGE_CURVE('',#5484,#5482,#1096,.T.);
#6657=EDGE_CURVE('',#5482,#5485,#4713,.T.);
#6658=EDGE_CURVE('',#5486,#5484,#4714,.T.);
#6659=EDGE_CURVE('',#5486,#5485,#1097,.T.);
#6660=EDGE_CURVE('',#5485,#5487,#1098,.T.);
#6661=EDGE_CURVE('',#5488,#5486,#1099,.T.);
#6662=EDGE_CURVE('',#5488,#5487,#1100,.T.);
#6663=EDGE_CURVE('',#5487,#5481,#4715,.T.);
#6664=EDGE_CURVE('',#5483,#5488,#4716,.T.);
#6665=EDGE_CURVE('',#5489,#5489,#4717,.T.);
#6666=EDGE_CURVE('',#5489,#5490,#1101,.T.);
#6667=EDGE_CURVE('',#5490,#5490,#4718,.T.);
#6668=EDGE_CURVE('',#5491,#5491,#4719,.T.);
#6669=EDGE_CURVE('',#5491,#5492,#1102,.T.);
#6670=EDGE_CURVE('',#5492,#5492,#4720,.T.);
#6671=EDGE_CURVE('',#5493,#5493,#4721,.T.);
#6672=EDGE_CURVE('',#5493,#5494,#1103,.T.);
#6673=EDGE_CURVE('',#5494,#5494,#4722,.T.);
#6674=EDGE_CURVE('',#5495,#5495,#4723,.T.);
#6675=EDGE_CURVE('',#5495,#5496,#1104,.T.);
#6676=EDGE_CURVE('',#5496,#5496,#4724,.T.);
#6677=EDGE_CURVE('',#5497,#5497,#4725,.T.);
#6678=EDGE_CURVE('',#5497,#5498,#1105,.T.);
#6679=EDGE_CURVE('',#5498,#5498,#4726,.T.);
#6680=EDGE_CURVE('',#5499,#5500,#1106,.T.);
#6681=EDGE_CURVE('',#5501,#5499,#1107,.T.);
#6682=EDGE_CURVE('',#5502,#5501,#1108,.T.);
#6683=EDGE_CURVE('',#5502,#5500,#1109,.T.);
#6684=EDGE_CURVE('',#5500,#5503,#4727,.T.);
#6685=EDGE_CURVE('',#5504,#5502,#4728,.T.);
#6686=EDGE_CURVE('',#5504,#5503,#1110,.T.);
#6687=EDGE_CURVE('',#5503,#5505,#1111,.T.);
#6688=EDGE_CURVE('',#5506,#5504,#1112,.T.);
#6689=EDGE_CURVE('',#5506,#5505,#1113,.T.);
#6690=EDGE_CURVE('',#5505,#5499,#4729,.T.);
#6691=EDGE_CURVE('',#5501,#5506,#4730,.T.);
#6692=EDGE_CURVE('',#5507,#5508,#1114,.T.);
#6693=EDGE_CURVE('',#5509,#5507,#1115,.T.);
#6694=EDGE_CURVE('',#5510,#5509,#1116,.T.);
#6695=EDGE_CURVE('',#5510,#5508,#1117,.T.);
#6696=EDGE_CURVE('',#5508,#5511,#4731,.T.);
#6697=EDGE_CURVE('',#5512,#5510,#4732,.T.);
#6698=EDGE_CURVE('',#5512,#5511,#1118,.T.);
#6699=EDGE_CURVE('',#5511,#5513,#1119,.T.);
#6700=EDGE_CURVE('',#5514,#5512,#1120,.T.);
#6701=EDGE_CURVE('',#5514,#5513,#1121,.T.);
#6702=EDGE_CURVE('',#5513,#5507,#4733,.T.);
#6703=EDGE_CURVE('',#5509,#5514,#4734,.T.);
#6704=EDGE_CURVE('',#5515,#5515,#4735,.T.);
#6705=EDGE_CURVE('',#5515,#5516,#1122,.T.);
#6706=EDGE_CURVE('',#5516,#5516,#4736,.T.);
#6707=EDGE_CURVE('',#5517,#5517,#4737,.T.);
#6708=EDGE_CURVE('',#5517,#5518,#1123,.T.);
#6709=EDGE_CURVE('',#5518,#5518,#4738,.T.);
#6710=EDGE_CURVE('',#5519,#5519,#4739,.T.);
#6711=EDGE_CURVE('',#5519,#5520,#1124,.T.);
#6712=EDGE_CURVE('',#5520,#5520,#4740,.T.);
#6713=EDGE_CURVE('',#5521,#5521,#4741,.T.);
#6714=EDGE_CURVE('',#5521,#5522,#1125,.T.);
#6715=EDGE_CURVE('',#5522,#5522,#4742,.T.);
#6716=EDGE_CURVE('',#5523,#5523,#4743,.T.);
#6717=EDGE_CURVE('',#5523,#5524,#1126,.T.);
#6718=EDGE_CURVE('',#5524,#5524,#4744,.T.);
#6719=EDGE_CURVE('',#5525,#5526,#1127,.T.);
#6720=EDGE_CURVE('',#5527,#5525,#1128,.T.);
#6721=EDGE_CURVE('',#5528,#5527,#1129,.T.);
#6722=EDGE_CURVE('',#5528,#5526,#1130,.T.);
#6723=EDGE_CURVE('',#5526,#5529,#4745,.T.);
#6724=EDGE_CURVE('',#5530,#5528,#4746,.T.);
#6725=EDGE_CURVE('',#5530,#5529,#1131,.T.);
#6726=EDGE_CURVE('',#5529,#5531,#1132,.T.);
#6727=EDGE_CURVE('',#5532,#5530,#1133,.T.);
#6728=EDGE_CURVE('',#5532,#5531,#1134,.T.);
#6729=EDGE_CURVE('',#5531,#5525,#4747,.T.);
#6730=EDGE_CURVE('',#5527,#5532,#4748,.T.);
#6731=EDGE_CURVE('',#5533,#5534,#1135,.T.);
#6732=EDGE_CURVE('',#5535,#5533,#1136,.T.);
#6733=EDGE_CURVE('',#5536,#5535,#1137,.T.);
#6734=EDGE_CURVE('',#5536,#5534,#1138,.T.);
#6735=EDGE_CURVE('',#5534,#5537,#4749,.T.);
#6736=EDGE_CURVE('',#5538,#5536,#4750,.T.);
#6737=EDGE_CURVE('',#5538,#5537,#1139,.T.);
#6738=EDGE_CURVE('',#5537,#5539,#1140,.T.);
#6739=EDGE_CURVE('',#5540,#5538,#1141,.T.);
#6740=EDGE_CURVE('',#5540,#5539,#1142,.T.);
#6741=EDGE_CURVE('',#5539,#5533,#4751,.T.);
#6742=EDGE_CURVE('',#5535,#5540,#4752,.T.);
#6743=EDGE_CURVE('',#5541,#5541,#4753,.T.);
#6744=EDGE_CURVE('',#5541,#5542,#1143,.T.);
#6745=EDGE_CURVE('',#5542,#5542,#4754,.T.);
#6746=EDGE_CURVE('',#5543,#5543,#4755,.T.);
#6747=EDGE_CURVE('',#5543,#5544,#1144,.T.);
#6748=EDGE_CURVE('',#5544,#5544,#4756,.T.);
#6749=EDGE_CURVE('',#5545,#5545,#4757,.T.);
#6750=EDGE_CURVE('',#5545,#5546,#1145,.T.);
#6751=EDGE_CURVE('',#5546,#5546,#4758,.T.);
#6752=EDGE_CURVE('',#5547,#5547,#4759,.T.);
#6753=EDGE_CURVE('',#5547,#5548,#1146,.T.);
#6754=EDGE_CURVE('',#5548,#5548,#4760,.T.);
#6755=EDGE_CURVE('',#5549,#5549,#4761,.T.);
#6756=EDGE_CURVE('',#5549,#5550,#1147,.T.);
#6757=EDGE_CURVE('',#5550,#5550,#4762,.T.);
#6758=EDGE_CURVE('',#5551,#5552,#1148,.T.);
#6759=EDGE_CURVE('',#5553,#5551,#1149,.T.);
#6760=EDGE_CURVE('',#5554,#5553,#1150,.T.);
#6761=EDGE_CURVE('',#5554,#5552,#1151,.T.);
#6762=EDGE_CURVE('',#5552,#5555,#4763,.T.);
#6763=EDGE_CURVE('',#5556,#5554,#4764,.T.);
#6764=EDGE_CURVE('',#5556,#5555,#1152,.T.);
#6765=EDGE_CURVE('',#5555,#5557,#1153,.T.);
#6766=EDGE_CURVE('',#5558,#5556,#1154,.T.);
#6767=EDGE_CURVE('',#5558,#5557,#1155,.T.);
#6768=EDGE_CURVE('',#5557,#5551,#4765,.T.);
#6769=EDGE_CURVE('',#5553,#5558,#4766,.T.);
#6770=EDGE_CURVE('',#5559,#5560,#1156,.T.);
#6771=EDGE_CURVE('',#5561,#5559,#1157,.T.);
#6772=EDGE_CURVE('',#5562,#5561,#1158,.T.);
#6773=EDGE_CURVE('',#5562,#5560,#1159,.T.);
#6774=EDGE_CURVE('',#5560,#5563,#4767,.T.);
#6775=EDGE_CURVE('',#5564,#5562,#4768,.T.);
#6776=EDGE_CURVE('',#5564,#5563,#1160,.T.);
#6777=EDGE_CURVE('',#5563,#5565,#1161,.T.);
#6778=EDGE_CURVE('',#5566,#5564,#1162,.T.);
#6779=EDGE_CURVE('',#5566,#5565,#1163,.T.);
#6780=EDGE_CURVE('',#5565,#5559,#4769,.T.);
#6781=EDGE_CURVE('',#5561,#5566,#4770,.T.);
#6782=EDGE_CURVE('',#5567,#5567,#4771,.T.);
#6783=EDGE_CURVE('',#5567,#5568,#1164,.T.);
#6784=EDGE_CURVE('',#5568,#5568,#4772,.T.);
#6785=EDGE_CURVE('',#5569,#5569,#4773,.T.);
#6786=EDGE_CURVE('',#5569,#5570,#1165,.T.);
#6787=EDGE_CURVE('',#5570,#5570,#4774,.T.);
#6788=EDGE_CURVE('',#5571,#5571,#4775,.T.);
#6789=EDGE_CURVE('',#5571,#5572,#1166,.T.);
#6790=EDGE_CURVE('',#5572,#5572,#4776,.T.);
#6791=EDGE_CURVE('',#5573,#5573,#4777,.T.);
#6792=EDGE_CURVE('',#5573,#5574,#1167,.T.);
#6793=EDGE_CURVE('',#5574,#5574,#4778,.T.);
#6794=EDGE_CURVE('',#5575,#5575,#4779,.T.);
#6795=EDGE_CURVE('',#5575,#5576,#1168,.T.);
#6796=EDGE_CURVE('',#5576,#5576,#4780,.T.);
#6797=EDGE_CURVE('',#5577,#5578,#1169,.T.);
#6798=EDGE_CURVE('',#5579,#5577,#1170,.T.);
#6799=EDGE_CURVE('',#5580,#5579,#1171,.T.);
#6800=EDGE_CURVE('',#5580,#5578,#1172,.T.);
#6801=EDGE_CURVE('',#5578,#5581,#4781,.T.);
#6802=EDGE_CURVE('',#5582,#5580,#4782,.T.);
#6803=EDGE_CURVE('',#5582,#5581,#1173,.T.);
#6804=EDGE_CURVE('',#5581,#5583,#1174,.T.);
#6805=EDGE_CURVE('',#5584,#5582,#1175,.T.);
#6806=EDGE_CURVE('',#5584,#5583,#1176,.T.);
#6807=EDGE_CURVE('',#5583,#5577,#4783,.T.);
#6808=EDGE_CURVE('',#5579,#5584,#4784,.T.);
#6809=EDGE_CURVE('',#5585,#5586,#1177,.T.);
#6810=EDGE_CURVE('',#5587,#5585,#1178,.T.);
#6811=EDGE_CURVE('',#5588,#5587,#1179,.T.);
#6812=EDGE_CURVE('',#5588,#5586,#1180,.T.);
#6813=EDGE_CURVE('',#5586,#5589,#4785,.T.);
#6814=EDGE_CURVE('',#5590,#5588,#4786,.T.);
#6815=EDGE_CURVE('',#5590,#5589,#1181,.T.);
#6816=EDGE_CURVE('',#5589,#5591,#1182,.T.);
#6817=EDGE_CURVE('',#5592,#5590,#1183,.T.);
#6818=EDGE_CURVE('',#5592,#5591,#1184,.T.);
#6819=EDGE_CURVE('',#5591,#5585,#4787,.T.);
#6820=EDGE_CURVE('',#5587,#5592,#4788,.T.);
#6821=EDGE_CURVE('',#5593,#5593,#4789,.T.);
#6822=EDGE_CURVE('',#5593,#5594,#1185,.T.);
#6823=EDGE_CURVE('',#5594,#5594,#4790,.T.);
#6824=EDGE_CURVE('',#5595,#5595,#4791,.T.);
#6825=EDGE_CURVE('',#5595,#5596,#1186,.T.);
#6826=EDGE_CURVE('',#5596,#5596,#4792,.T.);
#6827=EDGE_CURVE('',#5597,#5597,#4793,.T.);
#6828=EDGE_CURVE('',#5597,#5598,#1187,.T.);
#6829=EDGE_CURVE('',#5598,#5598,#4794,.T.);
#6830=EDGE_CURVE('',#5599,#5599,#4795,.T.);
#6831=EDGE_CURVE('',#5599,#5600,#1188,.T.);
#6832=EDGE_CURVE('',#5600,#5600,#4796,.T.);
#6833=EDGE_CURVE('',#5601,#5601,#4797,.T.);
#6834=EDGE_CURVE('',#5601,#5602,#1189,.T.);
#6835=EDGE_CURVE('',#5602,#5602,#4798,.T.);
#6836=EDGE_CURVE('',#5603,#5604,#1190,.T.);
#6837=EDGE_CURVE('',#5605,#5603,#1191,.T.);
#6838=EDGE_CURVE('',#5606,#5605,#1192,.T.);
#6839=EDGE_CURVE('',#5606,#5604,#1193,.T.);
#6840=EDGE_CURVE('',#5604,#5607,#4799,.T.);
#6841=EDGE_CURVE('',#5608,#5606,#4800,.T.);
#6842=EDGE_CURVE('',#5608,#5607,#1194,.T.);
#6843=EDGE_CURVE('',#5607,#5609,#1195,.T.);
#6844=EDGE_CURVE('',#5610,#5608,#1196,.T.);
#6845=EDGE_CURVE('',#5610,#5609,#1197,.T.);
#6846=EDGE_CURVE('',#5609,#5603,#4801,.T.);
#6847=EDGE_CURVE('',#5605,#5610,#4802,.T.);
#6848=EDGE_CURVE('',#5611,#5612,#1198,.T.);
#6849=EDGE_CURVE('',#5613,#5611,#1199,.T.);
#6850=EDGE_CURVE('',#5614,#5613,#1200,.T.);
#6851=EDGE_CURVE('',#5614,#5612,#1201,.T.);
#6852=EDGE_CURVE('',#5612,#5615,#4803,.T.);
#6853=EDGE_CURVE('',#5616,#5614,#4804,.T.);
#6854=EDGE_CURVE('',#5616,#5615,#1202,.T.);
#6855=EDGE_CURVE('',#5615,#5617,#1203,.T.);
#6856=EDGE_CURVE('',#5618,#5616,#1204,.T.);
#6857=EDGE_CURVE('',#5618,#5617,#1205,.T.);
#6858=EDGE_CURVE('',#5617,#5611,#4805,.T.);
#6859=EDGE_CURVE('',#5613,#5618,#4806,.T.);
#6860=EDGE_CURVE('',#5619,#5619,#4807,.T.);
#6861=EDGE_CURVE('',#5619,#5620,#1206,.T.);
#6862=EDGE_CURVE('',#5620,#5620,#4808,.T.);
#6863=EDGE_CURVE('',#5621,#5621,#4809,.T.);
#6864=EDGE_CURVE('',#5621,#5622,#1207,.T.);
#6865=EDGE_CURVE('',#5622,#5622,#4810,.T.);
#6866=EDGE_CURVE('',#5623,#5624,#1208,.T.);
#6867=EDGE_CURVE('',#5625,#5623,#1209,.T.);
#6868=EDGE_CURVE('',#5626,#5625,#1210,.T.);
#6869=EDGE_CURVE('',#5626,#5624,#1211,.T.);
#6870=EDGE_CURVE('',#5624,#5627,#4811,.T.);
#6871=EDGE_CURVE('',#5628,#5626,#4812,.T.);
#6872=EDGE_CURVE('',#5628,#5627,#1212,.T.);
#6873=EDGE_CURVE('',#5627,#5629,#1213,.T.);
#6874=EDGE_CURVE('',#5630,#5628,#1214,.T.);
#6875=EDGE_CURVE('',#5630,#5629,#1215,.T.);
#6876=EDGE_CURVE('',#5629,#5623,#4813,.T.);
#6877=EDGE_CURVE('',#5625,#5630,#4814,.T.);
#6878=EDGE_CURVE('',#5631,#5632,#1216,.T.);
#6879=EDGE_CURVE('',#5633,#5631,#1217,.T.);
#6880=EDGE_CURVE('',#5634,#5633,#1218,.T.);
#6881=EDGE_CURVE('',#5634,#5632,#1219,.T.);
#6882=EDGE_CURVE('',#5632,#5635,#4815,.T.);
#6883=EDGE_CURVE('',#5636,#5634,#4816,.T.);
#6884=EDGE_CURVE('',#5636,#5635,#1220,.T.);
#6885=EDGE_CURVE('',#5635,#5637,#1221,.T.);
#6886=EDGE_CURVE('',#5638,#5636,#1222,.T.);
#6887=EDGE_CURVE('',#5638,#5637,#1223,.T.);
#6888=EDGE_CURVE('',#5637,#5631,#4817,.T.);
#6889=EDGE_CURVE('',#5633,#5638,#4818,.T.);
#6890=EDGE_CURVE('',#5639,#5639,#4819,.T.);
#6891=EDGE_CURVE('',#5639,#5640,#1224,.T.);
#6892=EDGE_CURVE('',#5640,#5640,#4820,.T.);
#6893=EDGE_CURVE('',#5641,#5641,#4821,.T.);
#6894=EDGE_CURVE('',#5641,#5642,#1225,.T.);
#6895=EDGE_CURVE('',#5642,#5642,#4822,.T.);
#6896=EDGE_CURVE('',#5643,#5643,#4823,.T.);
#6897=EDGE_CURVE('',#5643,#5644,#1226,.T.);
#6898=EDGE_CURVE('',#5644,#5644,#4824,.T.);
#6899=EDGE_CURVE('',#5645,#5646,#4825,.T.);
#6900=EDGE_CURVE('',#5646,#5647,#1227,.T.);
#6901=EDGE_CURVE('',#5647,#5648,#4826,.T.);
#6902=EDGE_CURVE('',#5648,#5645,#1228,.T.);
#6903=EDGE_CURVE('',#5646,#5649,#1229,.T.);
#6904=EDGE_CURVE('',#5650,#5649,#1230,.T.);
#6905=EDGE_CURVE('',#5647,#5650,#1231,.T.);
#6906=EDGE_CURVE('',#5649,#5651,#4827,.T.);
#6907=EDGE_CURVE('',#5651,#5652,#1232,.T.);
#6908=EDGE_CURVE('',#5652,#5650,#4828,.T.);
#6909=EDGE_CURVE('',#5651,#5653,#1233,.T.);
#6910=EDGE_CURVE('',#5653,#5654,#1234,.T.);
#6911=EDGE_CURVE('',#5654,#5652,#1235,.T.);
#6912=EDGE_CURVE('',#5655,#5655,#4829,.T.);
#6913=EDGE_CURVE('',#5656,#5656,#4830,.T.);
#6914=EDGE_CURVE('',#5657,#5657,#4831,.T.);
#6915=EDGE_CURVE('',#5658,#5658,#4832,.T.);
#6916=EDGE_CURVE('',#5659,#5659,#4833,.T.);
#6917=EDGE_CURVE('',#5660,#5660,#4834,.T.);
#6918=EDGE_CURVE('',#5661,#5661,#4835,.T.);
#6919=EDGE_CURVE('',#5662,#5662,#4836,.T.);
#6920=EDGE_CURVE('',#5663,#5663,#4837,.T.);
#6921=EDGE_CURVE('',#5664,#5664,#4838,.T.);
#6922=EDGE_CURVE('',#5665,#5665,#4839,.T.);
#6923=EDGE_CURVE('',#5666,#5666,#4840,.T.);
#6924=EDGE_CURVE('',#5667,#5667,#4841,.T.);
#6925=EDGE_CURVE('',#5668,#5668,#4842,.T.);
#6926=EDGE_CURVE('',#5669,#5669,#4843,.T.);
#6927=EDGE_CURVE('',#5670,#5670,#4844,.T.);
#6928=EDGE_CURVE('',#5671,#5671,#4845,.T.);
#6929=EDGE_CURVE('',#5672,#5672,#4846,.T.);
#6930=EDGE_CURVE('',#5673,#5673,#4847,.T.);
#6931=EDGE_CURVE('',#5674,#5674,#4848,.T.);
#6932=EDGE_CURVE('',#5675,#5675,#4849,.T.);
#6933=EDGE_CURVE('',#5676,#5676,#4850,.T.);
#6934=EDGE_CURVE('',#5677,#5677,#4851,.T.);
#6935=EDGE_CURVE('',#5678,#5678,#4852,.T.);
#6936=EDGE_CURVE('',#5679,#5679,#4853,.T.);
#6937=EDGE_CURVE('',#5680,#5680,#4854,.T.);
#6938=EDGE_CURVE('',#5681,#5681,#4855,.T.);
#6939=EDGE_CURVE('',#5682,#5682,#4856,.T.);
#6940=EDGE_CURVE('',#5683,#5683,#4857,.T.);
#6941=EDGE_CURVE('',#5684,#5684,#4858,.T.);
#6942=EDGE_CURVE('',#5685,#5685,#4859,.T.);
#6943=EDGE_CURVE('',#5686,#5686,#4860,.T.);
#6944=EDGE_CURVE('',#5687,#5687,#4861,.T.);
#6945=EDGE_CURVE('',#5688,#5688,#4862,.T.);
#6946=EDGE_CURVE('',#5689,#5689,#4863,.T.);
#6947=EDGE_CURVE('',#5690,#5690,#4864,.T.);
#6948=EDGE_CURVE('',#5691,#5691,#4865,.T.);
#6949=EDGE_CURVE('',#5692,#5692,#4866,.T.);
#6950=EDGE_CURVE('',#5693,#5693,#4867,.T.);
#6951=EDGE_CURVE('',#5694,#5694,#4868,.T.);
#6952=EDGE_CURVE('',#5695,#5695,#4869,.T.);
#6953=EDGE_CURVE('',#5696,#5696,#4870,.T.);
#6954=EDGE_CURVE('',#5697,#5697,#4871,.T.);
#6955=EDGE_CURVE('',#5698,#5698,#4872,.T.);
#6956=EDGE_CURVE('',#5699,#5699,#4873,.T.);
#6957=EDGE_CURVE('',#5700,#5700,#4874,.T.);
#6958=EDGE_CURVE('',#5701,#5701,#4875,.T.);
#6959=EDGE_CURVE('',#5702,#5703,#4876,.T.);
#6960=EDGE_CURVE('',#5703,#5704,#1236,.T.);
#6961=EDGE_CURVE('',#5704,#5705,#4877,.T.);
#6962=EDGE_CURVE('',#5705,#5702,#1237,.T.);
#6963=EDGE_CURVE('',#5706,#5705,#1238,.T.);
#6964=EDGE_CURVE('',#5707,#5706,#1239,.T.);
#6965=EDGE_CURVE('',#5707,#5702,#1240,.T.);
#6966=EDGE_CURVE('',#5708,#5704,#1241,.T.);
#6967=EDGE_CURVE('',#5653,#5708,#1242,.T.);
#6968=EDGE_CURVE('',#5709,#5645,#1243,.T.);
#6969=EDGE_CURVE('',#5710,#5709,#1244,.T.);
#6970=EDGE_CURVE('',#5711,#5710,#1245,.T.);
#6971=EDGE_CURVE('',#5706,#5711,#4878,.T.);
#6972=EDGE_CURVE('',#5712,#5707,#4879,.T.);
#6973=EDGE_CURVE('',#5711,#5712,#1246,.T.);
#6974=EDGE_CURVE('',#5713,#5713,#4880,.T.);
#6975=EDGE_CURVE('',#5713,#5655,#1247,.T.);
#6976=EDGE_CURVE('',#5714,#5714,#4881,.T.);
#6977=EDGE_CURVE('',#5714,#5656,#1248,.T.);
#6978=EDGE_CURVE('',#5715,#5715,#4882,.T.);
#6979=EDGE_CURVE('',#5715,#5657,#1249,.T.);
#6980=EDGE_CURVE('',#5716,#5716,#4883,.T.);
#6981=EDGE_CURVE('',#5716,#5658,#1250,.T.);
#6982=EDGE_CURVE('',#5717,#5717,#4884,.T.);
#6983=EDGE_CURVE('',#5717,#5659,#1251,.T.);
#6984=EDGE_CURVE('',#5718,#5718,#4885,.T.);
#6985=EDGE_CURVE('',#5718,#5660,#1252,.T.);
#6986=EDGE_CURVE('',#5719,#5719,#4886,.T.);
#6987=EDGE_CURVE('',#5719,#5661,#1253,.T.);
#6988=EDGE_CURVE('',#5720,#5720,#4887,.T.);
#6989=EDGE_CURVE('',#5720,#5662,#1254,.T.);
#6990=EDGE_CURVE('',#5721,#5721,#4888,.T.);
#6991=EDGE_CURVE('',#5721,#5663,#1255,.T.);
#6992=EDGE_CURVE('',#5722,#5722,#4889,.T.);
#6993=EDGE_CURVE('',#5722,#5664,#1256,.T.);
#6994=EDGE_CURVE('',#5723,#5723,#4890,.T.);
#6995=EDGE_CURVE('',#5723,#5665,#1257,.T.);
#6996=EDGE_CURVE('',#5724,#5724,#4891,.T.);
#6997=EDGE_CURVE('',#5724,#5666,#1258,.T.);
#6998=EDGE_CURVE('',#5725,#5725,#4892,.T.);
#6999=EDGE_CURVE('',#5725,#5667,#1259,.T.);
#7000=EDGE_CURVE('',#5726,#5726,#4893,.T.);
#7001=EDGE_CURVE('',#5726,#5668,#1260,.T.);
#7002=EDGE_CURVE('',#5727,#5727,#4894,.T.);
#7003=EDGE_CURVE('',#5727,#5669,#1261,.T.);
#7004=EDGE_CURVE('',#5728,#5728,#4895,.T.);
#7005=EDGE_CURVE('',#5728,#5670,#1262,.T.);
#7006=EDGE_CURVE('',#5729,#5729,#4896,.T.);
#7007=EDGE_CURVE('',#5729,#5671,#1263,.T.);
#7008=EDGE_CURVE('',#5730,#5730,#4897,.T.);
#7009=EDGE_CURVE('',#5730,#5672,#1264,.T.);
#7010=EDGE_CURVE('',#5731,#5731,#4898,.T.);
#7011=EDGE_CURVE('',#5731,#5673,#1265,.T.);
#7012=EDGE_CURVE('',#5732,#5732,#4899,.T.);
#7013=EDGE_CURVE('',#5732,#5674,#1266,.T.);
#7014=EDGE_CURVE('',#5733,#5733,#4900,.T.);
#7015=EDGE_CURVE('',#5733,#5675,#1267,.T.);
#7016=EDGE_CURVE('',#5734,#5734,#4901,.T.);
#7017=EDGE_CURVE('',#5734,#5676,#1268,.T.);
#7018=EDGE_CURVE('',#5735,#5735,#4902,.T.);
#7019=EDGE_CURVE('',#5735,#5677,#1269,.T.);
#7020=EDGE_CURVE('',#5736,#5736,#4903,.T.);
#7021=EDGE_CURVE('',#5736,#5678,#1270,.T.);
#7022=EDGE_CURVE('',#5737,#5737,#4904,.T.);
#7023=EDGE_CURVE('',#5737,#5679,#1271,.T.);
#7024=EDGE_CURVE('',#5738,#5738,#4905,.T.);
#7025=EDGE_CURVE('',#5738,#5680,#1272,.T.);
#7026=EDGE_CURVE('',#5739,#5739,#4906,.T.);
#7027=EDGE_CURVE('',#5739,#5681,#1273,.T.);
#7028=EDGE_CURVE('',#5740,#5740,#4907,.T.);
#7029=EDGE_CURVE('',#5740,#5682,#1274,.T.);
#7030=EDGE_CURVE('',#5741,#5741,#4908,.T.);
#7031=EDGE_CURVE('',#5741,#5683,#1275,.T.);
#7032=EDGE_CURVE('',#5742,#5742,#4909,.T.);
#7033=EDGE_CURVE('',#5742,#5684,#1276,.T.);
#7034=EDGE_CURVE('',#5743,#5743,#4910,.T.);
#7035=EDGE_CURVE('',#5743,#5685,#1277,.T.);
#7036=EDGE_CURVE('',#5744,#5744,#4911,.T.);
#7037=EDGE_CURVE('',#5744,#5686,#1278,.T.);
#7038=EDGE_CURVE('',#5745,#5745,#4912,.T.);
#7039=EDGE_CURVE('',#5745,#5687,#1279,.T.);
#7040=EDGE_CURVE('',#5746,#5746,#4913,.T.);
#7041=EDGE_CURVE('',#5746,#5688,#1280,.T.);
#7042=EDGE_CURVE('',#5747,#5747,#4914,.T.);
#7043=EDGE_CURVE('',#5747,#5689,#1281,.T.);
#7044=EDGE_CURVE('',#5748,#5748,#4915,.T.);
#7045=EDGE_CURVE('',#5748,#5690,#1282,.T.);
#7046=EDGE_CURVE('',#5749,#5749,#4916,.T.);
#7047=EDGE_CURVE('',#5749,#5691,#1283,.T.);
#7048=EDGE_CURVE('',#5750,#5750,#4917,.T.);
#7049=EDGE_CURVE('',#5750,#5692,#1284,.T.);
#7050=EDGE_CURVE('',#5751,#5751,#4918,.T.);
#7051=EDGE_CURVE('',#5751,#5693,#1285,.T.);
#7052=EDGE_CURVE('',#5752,#5752,#4919,.T.);
#7053=EDGE_CURVE('',#5752,#5694,#1286,.T.);
#7054=EDGE_CURVE('',#5753,#5753,#4920,.T.);
#7055=EDGE_CURVE('',#5753,#5695,#1287,.T.);
#7056=EDGE_CURVE('',#5754,#5754,#4921,.T.);
#7057=EDGE_CURVE('',#5754,#5696,#1288,.T.);
#7058=EDGE_CURVE('',#5755,#5755,#4922,.T.);
#7059=EDGE_CURVE('',#5755,#5697,#1289,.T.);
#7060=EDGE_CURVE('',#5756,#5756,#4923,.T.);
#7061=EDGE_CURVE('',#5756,#5698,#1290,.T.);
#7062=EDGE_CURVE('',#5757,#5757,#4924,.T.);
#7063=EDGE_CURVE('',#5757,#5699,#1291,.T.);
#7064=EDGE_CURVE('',#5758,#5758,#4925,.T.);
#7065=EDGE_CURVE('',#5758,#5700,#1292,.T.);
#7066=EDGE_CURVE('',#5759,#5759,#4926,.T.);
#7067=EDGE_CURVE('',#5759,#5701,#1293,.T.);
#7068=EDGE_CURVE('',#5760,#5708,#1294,.T.);
#7069=EDGE_CURVE('',#5654,#5760,#1295,.T.);
#7070=EDGE_CURVE('',#5703,#5760,#1296,.T.);
#7071=EDGE_CURVE('',#5761,#5761,#4927,.T.);
#7072=EDGE_CURVE('',#5761,#5762,#1297,.T.);
#7073=EDGE_CURVE('',#5762,#5762,#4928,.T.);
#7074=EDGE_CURVE('',#5763,#5763,#4929,.T.);
#7075=EDGE_CURVE('',#5763,#5764,#1298,.T.);
#7076=EDGE_CURVE('',#5764,#5764,#4930,.T.);
#7077=EDGE_CURVE('',#5765,#5765,#4931,.T.);
#7078=EDGE_CURVE('',#5765,#5766,#1299,.T.);
#7079=EDGE_CURVE('',#5766,#5766,#4932,.T.);
#7080=EDGE_CURVE('',#5767,#5767,#4933,.T.);
#7081=EDGE_CURVE('',#5767,#5768,#1300,.T.);
#7082=EDGE_CURVE('',#5768,#5768,#4934,.T.);
#7083=EDGE_CURVE('',#5769,#5769,#4935,.T.);
#7084=EDGE_CURVE('',#5769,#5770,#1301,.T.);
#7085=EDGE_CURVE('',#5770,#5770,#4936,.T.);
#7086=EDGE_CURVE('',#5771,#5771,#4937,.T.);
#7087=EDGE_CURVE('',#5771,#5772,#1302,.T.);
#7088=EDGE_CURVE('',#5772,#5772,#4938,.T.);
#7089=EDGE_CURVE('',#5773,#5773,#4939,.T.);
#7090=EDGE_CURVE('',#5773,#5774,#1303,.T.);
#7091=EDGE_CURVE('',#5774,#5774,#4940,.T.);
#7092=EDGE_CURVE('',#5775,#5775,#4941,.T.);
#7093=EDGE_CURVE('',#5775,#5776,#1304,.T.);
#7094=EDGE_CURVE('',#5776,#5776,#4942,.T.);
#7095=EDGE_CURVE('',#5777,#5777,#4943,.T.);
#7096=EDGE_CURVE('',#5777,#5778,#1305,.T.);
#7097=EDGE_CURVE('',#5778,#5778,#4944,.T.);
#7098=EDGE_CURVE('',#5779,#5779,#4945,.T.);
#7099=EDGE_CURVE('',#5779,#5780,#1306,.T.);
#7100=EDGE_CURVE('',#5780,#5780,#4946,.T.);
#7101=EDGE_CURVE('',#5781,#5781,#4947,.T.);
#7102=EDGE_CURVE('',#5781,#5782,#1307,.T.);
#7103=EDGE_CURVE('',#5782,#5782,#4948,.T.);
#7104=EDGE_CURVE('',#5783,#5783,#4949,.T.);
#7105=EDGE_CURVE('',#5783,#5784,#1308,.T.);
#7106=EDGE_CURVE('',#5784,#5784,#4950,.T.);
#7107=EDGE_CURVE('',#5785,#5785,#4951,.T.);
#7108=EDGE_CURVE('',#5785,#5786,#1309,.T.);
#7109=EDGE_CURVE('',#5786,#5786,#4952,.T.);
#7110=EDGE_CURVE('',#5787,#5787,#4953,.T.);
#7111=EDGE_CURVE('',#5787,#5788,#1310,.T.);
#7112=EDGE_CURVE('',#5788,#5788,#4954,.T.);
#7113=EDGE_CURVE('',#5789,#5789,#4955,.T.);
#7114=EDGE_CURVE('',#5789,#5790,#1311,.T.);
#7115=EDGE_CURVE('',#5790,#5790,#4956,.T.);
#7116=EDGE_CURVE('',#5791,#5791,#4957,.T.);
#7117=EDGE_CURVE('',#5791,#5792,#1312,.T.);
#7118=EDGE_CURVE('',#5792,#5792,#4958,.T.);
#7119=EDGE_CURVE('',#5793,#5793,#4959,.T.);
#7120=EDGE_CURVE('',#5793,#5794,#1313,.T.);
#7121=EDGE_CURVE('',#5794,#5794,#4960,.T.);
#7122=EDGE_CURVE('',#5795,#5795,#4961,.T.);
#7123=EDGE_CURVE('',#5795,#5796,#1314,.T.);
#7124=EDGE_CURVE('',#5796,#5796,#4962,.T.);
#7125=EDGE_CURVE('',#5797,#5797,#4963,.T.);
#7126=EDGE_CURVE('',#5797,#5798,#1315,.T.);
#7127=EDGE_CURVE('',#5798,#5798,#4964,.T.);
#7128=EDGE_CURVE('',#5799,#5799,#4965,.T.);
#7129=EDGE_CURVE('',#5799,#5800,#1316,.T.);
#7130=EDGE_CURVE('',#5800,#5800,#4966,.T.);
#7131=EDGE_CURVE('',#5801,#5801,#4967,.T.);
#7132=EDGE_CURVE('',#5801,#5802,#1317,.T.);
#7133=EDGE_CURVE('',#5802,#5802,#4968,.T.);
#7134=EDGE_CURVE('',#5803,#5803,#4969,.T.);
#7135=EDGE_CURVE('',#5803,#5804,#1318,.T.);
#7136=EDGE_CURVE('',#5804,#5804,#4970,.T.);
#7137=EDGE_CURVE('',#5805,#5805,#4971,.T.);
#7138=EDGE_CURVE('',#5805,#5806,#1319,.T.);
#7139=EDGE_CURVE('',#5806,#5806,#4972,.T.);
#7140=EDGE_CURVE('',#5807,#5807,#4973,.T.);
#7141=EDGE_CURVE('',#5807,#5808,#1320,.T.);
#7142=EDGE_CURVE('',#5808,#5808,#4974,.T.);
#7143=EDGE_CURVE('',#5809,#5809,#4975,.T.);
#7144=EDGE_CURVE('',#5809,#5810,#1321,.T.);
#7145=EDGE_CURVE('',#5810,#5810,#4976,.T.);
#7146=EDGE_CURVE('',#5811,#5811,#4977,.T.);
#7147=EDGE_CURVE('',#5811,#5812,#1322,.T.);
#7148=EDGE_CURVE('',#5812,#5812,#4978,.T.);
#7149=EDGE_CURVE('',#5813,#5813,#4979,.T.);
#7150=EDGE_CURVE('',#5813,#5814,#1323,.T.);
#7151=EDGE_CURVE('',#5814,#5814,#4980,.T.);
#7152=EDGE_CURVE('',#5815,#5815,#4981,.T.);
#7153=EDGE_CURVE('',#5815,#5816,#1324,.T.);
#7154=EDGE_CURVE('',#5816,#5816,#4982,.T.);
#7155=EDGE_CURVE('',#5817,#5817,#4983,.T.);
#7156=EDGE_CURVE('',#5817,#5818,#1325,.T.);
#7157=EDGE_CURVE('',#5818,#5818,#4984,.T.);
#7158=EDGE_CURVE('',#5819,#5819,#4985,.T.);
#7159=EDGE_CURVE('',#5819,#5820,#1326,.T.);
#7160=EDGE_CURVE('',#5820,#5820,#4986,.T.);
#7161=EDGE_CURVE('',#5821,#5821,#4987,.T.);
#7162=EDGE_CURVE('',#5821,#5822,#1327,.T.);
#7163=EDGE_CURVE('',#5822,#5822,#4988,.T.);
#7164=EDGE_CURVE('',#5823,#5823,#4989,.T.);
#7165=EDGE_CURVE('',#5823,#5824,#1328,.T.);
#7166=EDGE_CURVE('',#5824,#5824,#4990,.T.);
#7167=EDGE_CURVE('',#5825,#5825,#4991,.T.);
#7168=EDGE_CURVE('',#5825,#5826,#1329,.T.);
#7169=EDGE_CURVE('',#5826,#5826,#4992,.T.);
#7170=EDGE_CURVE('',#5827,#5827,#4993,.T.);
#7171=EDGE_CURVE('',#5827,#5828,#1330,.T.);
#7172=EDGE_CURVE('',#5828,#5828,#4994,.T.);
#7173=EDGE_CURVE('',#5829,#5829,#4995,.T.);
#7174=EDGE_CURVE('',#5829,#5830,#1331,.T.);
#7175=EDGE_CURVE('',#5830,#5830,#4996,.T.);
#7176=EDGE_CURVE('',#5831,#5831,#4997,.T.);
#7177=EDGE_CURVE('',#5831,#5832,#1332,.T.);
#7178=EDGE_CURVE('',#5832,#5832,#4998,.T.);
#7179=EDGE_CURVE('',#5833,#5833,#4999,.T.);
#7180=EDGE_CURVE('',#5833,#5834,#1333,.T.);
#7181=EDGE_CURVE('',#5834,#5834,#5000,.T.);
#7182=EDGE_CURVE('',#5835,#5835,#5001,.T.);
#7183=EDGE_CURVE('',#5835,#5836,#1334,.T.);
#7184=EDGE_CURVE('',#5836,#5836,#5002,.T.);
#7185=EDGE_CURVE('',#5837,#5837,#5003,.T.);
#7186=EDGE_CURVE('',#5837,#5838,#1335,.T.);
#7187=EDGE_CURVE('',#5838,#5838,#5004,.T.);
#7188=EDGE_CURVE('',#5839,#5839,#5005,.T.);
#7189=EDGE_CURVE('',#5839,#5840,#1336,.T.);
#7190=EDGE_CURVE('',#5840,#5840,#5006,.T.);
#7191=EDGE_CURVE('',#5841,#5841,#5007,.T.);
#7192=EDGE_CURVE('',#5841,#5842,#1337,.T.);
#7193=EDGE_CURVE('',#5842,#5842,#5008,.T.);
#7194=EDGE_CURVE('',#5843,#5843,#5009,.T.);
#7195=EDGE_CURVE('',#5843,#5844,#1338,.T.);
#7196=EDGE_CURVE('',#5844,#5844,#5010,.T.);
#7197=EDGE_CURVE('',#5845,#5845,#5011,.T.);
#7198=EDGE_CURVE('',#5845,#5846,#1339,.T.);
#7199=EDGE_CURVE('',#5846,#5846,#5012,.T.);
#7200=EDGE_CURVE('',#5847,#5847,#5013,.T.);
#7201=EDGE_CURVE('',#5847,#5848,#1340,.T.);
#7202=EDGE_CURVE('',#5848,#5848,#5014,.T.);
#7203=EDGE_CURVE('',#5849,#5849,#5015,.T.);
#7204=EDGE_CURVE('',#5849,#5850,#1341,.T.);
#7205=EDGE_CURVE('',#5850,#5850,#5016,.T.);
#7206=EDGE_CURVE('',#5851,#5851,#5017,.T.);
#7207=EDGE_CURVE('',#5851,#5852,#1342,.T.);
#7208=EDGE_CURVE('',#5852,#5852,#5018,.T.);
#7209=EDGE_CURVE('',#5853,#5853,#5019,.T.);
#7210=EDGE_CURVE('',#5853,#5854,#1343,.T.);
#7211=EDGE_CURVE('',#5854,#5854,#5020,.T.);
#7212=EDGE_CURVE('',#5710,#5855,#1344,.T.);
#7213=EDGE_CURVE('',#5856,#5709,#1345,.T.);
#7214=EDGE_CURVE('',#5855,#5856,#1346,.T.);
#7215=EDGE_CURVE('',#5855,#5712,#1347,.T.);
#7216=EDGE_CURVE('',#5648,#5856,#1348,.T.);
#7217=EDGE_CURVE('',#5857,#5857,#5021,.T.);
#7218=EDGE_CURVE('',#5857,#5858,#1349,.T.);
#7219=EDGE_CURVE('',#5858,#5858,#5022,.T.);
#7220=EDGE_CURVE('',#5859,#5859,#5023,.T.);
#7221=EDGE_CURVE('',#5859,#5860,#1350,.T.);
#7222=EDGE_CURVE('',#5860,#5860,#5024,.T.);
#7223=EDGE_CURVE('',#5861,#5861,#5025,.T.);
#7224=EDGE_CURVE('',#5861,#5862,#1351,.T.);
#7225=EDGE_CURVE('',#5862,#5862,#5026,.T.);
#7226=EDGE_CURVE('',#5863,#5864,#5027,.T.);
#7227=EDGE_CURVE('',#5864,#5865,#1352,.T.);
#7228=EDGE_CURVE('',#5865,#5866,#5028,.T.);
#7229=EDGE_CURVE('',#5866,#5863,#1353,.T.);
#7230=EDGE_CURVE('',#5864,#5867,#1354,.T.);
#7231=EDGE_CURVE('',#5868,#5867,#1355,.T.);
#7232=EDGE_CURVE('',#5868,#5869,#1356,.T.);
#7233=EDGE_CURVE('',#5869,#5870,#1357,.T.);
#7234=EDGE_CURVE('',#5871,#5870,#1358,.T.);
#7235=EDGE_CURVE('',#5871,#5872,#1359,.T.);
#7236=EDGE_CURVE('',#5872,#5865,#1360,.T.);
#7237=EDGE_CURVE('',#5873,#5873,#5029,.T.);
#7238=EDGE_CURVE('',#5874,#5874,#5030,.T.);
#7239=EDGE_CURVE('',#5875,#5875,#5031,.T.);
#7240=EDGE_CURVE('',#5876,#5876,#5032,.T.);
#7241=EDGE_CURVE('',#5877,#5877,#5033,.T.);
#7242=EDGE_CURVE('',#5878,#5878,#5034,.T.);
#7243=EDGE_CURVE('',#5879,#5879,#5035,.T.);
#7244=EDGE_CURVE('',#5880,#5880,#5036,.T.);
#7245=EDGE_CURVE('',#5881,#5881,#5037,.T.);
#7246=EDGE_CURVE('',#5882,#5882,#5038,.T.);
#7247=EDGE_CURVE('',#5883,#5883,#5039,.T.);
#7248=EDGE_CURVE('',#5884,#5885,#5040,.T.);
#7249=EDGE_CURVE('',#5885,#5886,#1361,.T.);
#7250=EDGE_CURVE('',#5886,#5887,#5041,.T.);
#7251=EDGE_CURVE('',#5884,#5887,#1362,.T.);
#7252=EDGE_CURVE('',#5885,#5888,#1363,.T.);
#7253=EDGE_CURVE('',#5888,#5889,#1364,.T.);
#7254=EDGE_CURVE('',#5889,#5890,#1365,.T.);
#7255=EDGE_CURVE('',#5890,#5891,#1366,.T.);
#7256=EDGE_CURVE('',#5891,#5892,#1367,.T.);
#7257=EDGE_CURVE('',#5892,#5893,#1368,.T.);
#7258=EDGE_CURVE('',#5893,#5886,#1369,.T.);
#7259=EDGE_CURVE('',#5894,#5894,#5042,.T.);
#7260=EDGE_CURVE('',#5895,#5895,#5043,.T.);
#7261=EDGE_CURVE('',#5896,#5896,#5044,.T.);
#7262=EDGE_CURVE('',#5897,#5897,#5045,.T.);
#7263=EDGE_CURVE('',#5898,#5898,#5046,.T.);
#7264=EDGE_CURVE('',#5899,#5899,#5047,.T.);
#7265=EDGE_CURVE('',#5900,#5900,#5048,.T.);
#7266=EDGE_CURVE('',#5901,#5901,#5049,.T.);
#7267=EDGE_CURVE('',#5902,#5902,#5050,.T.);
#7268=EDGE_CURVE('',#5903,#5903,#5051,.T.);
#7269=EDGE_CURVE('',#5904,#5904,#5052,.T.);
#7270=EDGE_CURVE('',#5894,#5883,#1370,.T.);
#7271=EDGE_CURVE('',#5895,#5882,#1371,.T.);
#7272=EDGE_CURVE('',#5896,#5881,#1372,.T.);
#7273=EDGE_CURVE('',#5897,#5880,#1373,.T.);
#7274=EDGE_CURVE('',#5898,#5879,#1374,.T.);
#7275=EDGE_CURVE('',#5899,#5878,#1375,.T.);
#7276=EDGE_CURVE('',#5900,#5877,#1376,.T.);
#7277=EDGE_CURVE('',#5901,#5876,#1377,.T.);
#7278=EDGE_CURVE('',#5902,#5875,#1378,.T.);
#7279=EDGE_CURVE('',#5903,#5874,#1379,.T.);
#7280=EDGE_CURVE('',#5904,#5873,#1380,.T.);
#7281=EDGE_CURVE('',#5871,#5889,#1381,.T.);
#7282=EDGE_CURVE('',#5872,#5888,#1382,.T.);
#7283=EDGE_CURVE('',#5867,#5893,#1383,.T.);
#7284=EDGE_CURVE('',#5868,#5892,#1384,.T.);
#7285=EDGE_CURVE('',#5869,#5891,#1385,.T.);
#7286=EDGE_CURVE('',#5870,#5890,#1386,.T.);
#7287=EDGE_CURVE('',#5905,#5906,#1387,.T.);
#7288=EDGE_CURVE('',#5905,#5907,#1388,.T.);
#7289=EDGE_CURVE('',#5908,#5907,#1389,.T.);
#7290=EDGE_CURVE('',#5908,#5909,#1390,.T.);
#7291=EDGE_CURVE('',#5909,#5910,#1391,.T.);
#7292=EDGE_CURVE('',#5911,#5910,#1392,.T.);
#7293=EDGE_CURVE('',#5911,#5912,#1393,.T.);
#7294=EDGE_CURVE('',#5912,#5906,#1394,.T.);
#7295=EDGE_CURVE('',#5913,#5913,#5053,.T.);
#7296=EDGE_CURVE('',#5914,#5914,#5054,.T.);
#7297=EDGE_CURVE('',#5915,#5915,#5055,.T.);
#7298=EDGE_CURVE('',#5916,#5916,#5056,.T.);
#7299=EDGE_CURVE('',#5917,#5917,#5057,.T.);
#7300=EDGE_CURVE('',#5918,#5918,#5058,.T.);
#7301=EDGE_CURVE('',#5919,#5919,#5059,.T.);
#7302=EDGE_CURVE('',#5920,#5920,#5060,.T.);
#7303=EDGE_CURVE('',#5921,#5921,#5061,.T.);
#7304=EDGE_CURVE('',#5922,#5922,#5062,.T.);
#7305=EDGE_CURVE('',#5923,#5923,#5063,.T.);
#7306=EDGE_CURVE('',#5924,#5924,#5064,.T.);
#7307=EDGE_CURVE('',#5924,#5913,#1395,.T.);
#7308=EDGE_CURVE('',#5925,#5925,#5065,.T.);
#7309=EDGE_CURVE('',#5925,#5914,#1396,.T.);
#7310=EDGE_CURVE('',#5926,#5926,#5066,.T.);
#7311=EDGE_CURVE('',#5926,#5915,#1397,.T.);
#7312=EDGE_CURVE('',#5927,#5927,#5067,.T.);
#7313=EDGE_CURVE('',#5927,#5916,#1398,.T.);
#7314=EDGE_CURVE('',#5928,#5928,#5068,.T.);
#7315=EDGE_CURVE('',#5928,#5917,#1399,.T.);
#7316=EDGE_CURVE('',#5929,#5929,#5069,.T.);
#7317=EDGE_CURVE('',#5929,#5918,#1400,.T.);
#7318=EDGE_CURVE('',#5930,#5930,#5070,.T.);
#7319=EDGE_CURVE('',#5930,#5919,#1401,.T.);
#7320=EDGE_CURVE('',#5931,#5931,#5071,.T.);
#7321=EDGE_CURVE('',#5931,#5920,#1402,.T.);
#7322=EDGE_CURVE('',#5932,#5932,#5072,.T.);
#7323=EDGE_CURVE('',#5932,#5921,#1403,.T.);
#7324=EDGE_CURVE('',#5933,#5933,#5073,.T.);
#7325=EDGE_CURVE('',#5933,#5922,#1404,.T.);
#7326=EDGE_CURVE('',#5934,#5934,#5074,.T.);
#7327=EDGE_CURVE('',#5934,#5923,#1405,.T.);
#7328=EDGE_CURVE('',#5911,#5935,#1406,.T.);
#7329=EDGE_CURVE('',#5936,#5935,#1407,.T.);
#7330=EDGE_CURVE('',#5912,#5936,#1408,.T.);
#7331=EDGE_CURVE('',#5907,#5937,#1409,.T.);
#7332=EDGE_CURVE('',#5938,#5937,#1410,.T.);
#7333=EDGE_CURVE('',#5908,#5938,#1411,.T.);
#7334=EDGE_CURVE('',#5939,#5938,#1412,.T.);
#7335=EDGE_CURVE('',#5909,#5939,#1413,.T.);
#7336=EDGE_CURVE('',#5940,#5939,#1414,.T.);
#7337=EDGE_CURVE('',#5910,#5940,#1415,.T.);
#7338=EDGE_CURVE('',#5935,#5940,#1416,.T.);
#7339=EDGE_CURVE('',#5941,#5942,#1417,.T.);
#7340=EDGE_CURVE('',#5941,#5936,#1418,.T.);
#7341=EDGE_CURVE('',#5937,#5942,#1419,.T.);
#7342=EDGE_CURVE('',#5884,#5943,#1420,.T.);
#7343=EDGE_CURVE('',#5887,#5944,#1421,.T.);
#7344=EDGE_CURVE('',#5943,#5944,#1422,.T.);
#7345=EDGE_CURVE('',#5866,#5941,#1423,.T.);
#7346=EDGE_CURVE('',#5863,#5942,#1424,.T.);
#7347=EDGE_CURVE('',#5945,#5943,#1425,.T.);
#7348=EDGE_CURVE('',#5906,#5945,#1426,.T.);
#7349=EDGE_CURVE('',#5946,#5945,#1427,.T.);
#7350=EDGE_CURVE('',#5905,#5946,#1428,.T.);
#7351=EDGE_CURVE('',#5944,#5946,#1429,.T.);
#7352=EDGE_CURVE('',#5947,#5947,#5075,.T.);
#7353=EDGE_CURVE('',#5947,#5948,#1430,.T.);
#7354=EDGE_CURVE('',#5948,#5948,#5076,.F.);
#7355=EDGE_CURVE('',#5949,#5950,#1431,.T.);
#7356=EDGE_CURVE('',#5949,#5951,#1432,.T.);
#7357=EDGE_CURVE('',#5952,#5951,#1433,.T.);
#7358=EDGE_CURVE('',#5950,#5952,#1434,.T.);
#7359=EDGE_CURVE('',#5950,#5953,#1435,.T.);
#7360=EDGE_CURVE('',#5954,#5952,#1436,.T.);
#7361=EDGE_CURVE('',#5953,#5954,#1437,.T.);
#7362=EDGE_CURVE('',#5953,#5955,#1438,.T.);
#7363=EDGE_CURVE('',#5956,#5954,#1439,.T.);
#7364=EDGE_CURVE('',#5955,#5956,#1440,.T.);
#7365=EDGE_CURVE('',#5955,#5957,#1441,.T.);
#7366=EDGE_CURVE('',#5958,#5956,#1442,.T.);
#7367=EDGE_CURVE('',#5957,#5958,#1443,.T.);
#7368=EDGE_CURVE('',#5957,#5959,#1444,.T.);
#7369=EDGE_CURVE('',#5960,#5958,#1445,.T.);
#7370=EDGE_CURVE('',#5959,#5960,#1446,.T.);
#7371=EDGE_CURVE('',#5959,#5949,#1447,.T.);
#7372=EDGE_CURVE('',#5951,#5960,#1448,.T.);
#7373=EDGE_CURVE('',#5961,#5961,#5077,.T.);
#7374=EDGE_CURVE('',#5961,#5962,#1449,.T.);
#7375=EDGE_CURVE('',#5962,#5962,#5078,.T.);
#7376=EDGE_CURVE('',#5963,#5963,#5079,.T.);
#7377=EDGE_CURVE('',#5963,#5964,#1450,.T.);
#7378=EDGE_CURVE('',#5964,#5964,#5080,.T.);
#7379=EDGE_CURVE('',#5965,#5965,#5081,.T.);
#7380=EDGE_CURVE('',#5965,#5966,#1451,.T.);
#7381=EDGE_CURVE('',#5966,#5966,#5082,.T.);
#7382=EDGE_CURVE('',#5967,#5968,#5083,.T.);
#7383=EDGE_CURVE('',#5968,#5969,#1452,.T.);
#7384=EDGE_CURVE('',#5969,#5970,#5084,.T.);
#7385=EDGE_CURVE('',#5970,#5967,#1453,.T.);
#7386=EDGE_CURVE('',#5968,#5971,#1454,.T.);
#7387=EDGE_CURVE('',#5972,#5971,#1455,.T.);
#7388=EDGE_CURVE('',#5972,#5973,#1456,.T.);
#7389=EDGE_CURVE('',#5973,#5974,#1457,.T.);
#7390=EDGE_CURVE('',#5975,#5974,#1458,.T.);
#7391=EDGE_CURVE('',#5975,#5976,#1459,.T.);
#7392=EDGE_CURVE('',#5976,#5969,#1460,.T.);
#7393=EDGE_CURVE('',#5977,#5977,#5085,.T.);
#7394=EDGE_CURVE('',#5978,#5978,#5086,.T.);
#7395=EDGE_CURVE('',#5979,#5979,#5087,.T.);
#7396=EDGE_CURVE('',#5980,#5980,#5088,.T.);
#7397=EDGE_CURVE('',#5981,#5981,#5089,.T.);
#7398=EDGE_CURVE('',#5982,#5982,#5090,.T.);
#7399=EDGE_CURVE('',#5983,#5983,#5091,.T.);
#7400=EDGE_CURVE('',#5984,#5984,#5092,.T.);
#7401=EDGE_CURVE('',#5985,#5985,#5093,.T.);
#7402=EDGE_CURVE('',#5986,#5986,#5094,.T.);
#7403=EDGE_CURVE('',#5987,#5987,#5095,.T.);
#7404=EDGE_CURVE('',#5988,#5989,#5096,.T.);
#7405=EDGE_CURVE('',#5989,#5990,#1461,.T.);
#7406=EDGE_CURVE('',#5990,#5991,#5097,.T.);
#7407=EDGE_CURVE('',#5988,#5991,#1462,.T.);
#7408=EDGE_CURVE('',#5989,#5992,#1463,.T.);
#7409=EDGE_CURVE('',#5992,#5993,#1464,.T.);
#7410=EDGE_CURVE('',#5993,#5994,#1465,.T.);
#7411=EDGE_CURVE('',#5994,#5995,#1466,.T.);
#7412=EDGE_CURVE('',#5995,#5996,#1467,.T.);
#7413=EDGE_CURVE('',#5996,#5997,#1468,.T.);
#7414=EDGE_CURVE('',#5997,#5990,#1469,.T.);
#7415=EDGE_CURVE('',#5998,#5998,#5098,.T.);
#7416=EDGE_CURVE('',#5999,#5999,#5099,.T.);
#7417=EDGE_CURVE('',#6000,#6000,#5100,.T.);
#7418=EDGE_CURVE('',#6001,#6001,#5101,.T.);
#7419=EDGE_CURVE('',#6002,#6002,#5102,.T.);
#7420=EDGE_CURVE('',#6003,#6003,#5103,.T.);
#7421=EDGE_CURVE('',#6004,#6004,#5104,.T.);
#7422=EDGE_CURVE('',#6005,#6005,#5105,.T.);
#7423=EDGE_CURVE('',#6006,#6006,#5106,.T.);
#7424=EDGE_CURVE('',#6007,#6007,#5107,.T.);
#7425=EDGE_CURVE('',#6008,#6008,#5108,.T.);
#7426=EDGE_CURVE('',#5998,#5987,#1470,.T.);
#7427=EDGE_CURVE('',#5999,#5986,#1471,.T.);
#7428=EDGE_CURVE('',#6000,#5985,#1472,.T.);
#7429=EDGE_CURVE('',#6001,#5984,#1473,.T.);
#7430=EDGE_CURVE('',#6002,#5983,#1474,.T.);
#7431=EDGE_CURVE('',#6003,#5982,#1475,.T.);
#7432=EDGE_CURVE('',#6004,#5981,#1476,.T.);
#7433=EDGE_CURVE('',#6005,#5980,#1477,.T.);
#7434=EDGE_CURVE('',#6006,#5979,#1478,.T.);
#7435=EDGE_CURVE('',#6007,#5978,#1479,.T.);
#7436=EDGE_CURVE('',#6008,#5977,#1480,.T.);
#7437=EDGE_CURVE('',#5975,#5993,#1481,.T.);
#7438=EDGE_CURVE('',#5976,#5992,#1482,.T.);
#7439=EDGE_CURVE('',#5971,#5997,#1483,.T.);
#7440=EDGE_CURVE('',#5972,#5996,#1484,.T.);
#7441=EDGE_CURVE('',#5973,#5995,#1485,.T.);
#7442=EDGE_CURVE('',#5974,#5994,#1486,.T.);
#7443=EDGE_CURVE('',#6009,#6010,#1487,.T.);
#7444=EDGE_CURVE('',#6009,#6011,#1488,.T.);
#7445=EDGE_CURVE('',#6012,#6011,#1489,.T.);
#7446=EDGE_CURVE('',#6012,#6013,#1490,.T.);
#7447=EDGE_CURVE('',#6013,#6014,#1491,.T.);
#7448=EDGE_CURVE('',#6015,#6014,#1492,.T.);
#7449=EDGE_CURVE('',#6015,#6016,#1493,.T.);
#7450=EDGE_CURVE('',#6016,#6010,#1494,.T.);
#7451=EDGE_CURVE('',#6017,#6017,#5109,.T.);
#7452=EDGE_CURVE('',#6018,#6018,#5110,.T.);
#7453=EDGE_CURVE('',#6019,#6019,#5111,.T.);
#7454=EDGE_CURVE('',#6020,#6020,#5112,.T.);
#7455=EDGE_CURVE('',#6021,#6021,#5113,.T.);
#7456=EDGE_CURVE('',#6022,#6022,#5114,.T.);
#7457=EDGE_CURVE('',#6023,#6023,#5115,.T.);
#7458=EDGE_CURVE('',#6024,#6024,#5116,.T.);
#7459=EDGE_CURVE('',#6025,#6025,#5117,.T.);
#7460=EDGE_CURVE('',#6026,#6026,#5118,.T.);
#7461=EDGE_CURVE('',#6027,#6027,#5119,.T.);
#7462=EDGE_CURVE('',#6028,#6028,#5120,.T.);
#7463=EDGE_CURVE('',#6028,#6017,#1495,.T.);
#7464=EDGE_CURVE('',#6029,#6029,#5121,.T.);
#7465=EDGE_CURVE('',#6029,#6018,#1496,.T.);
#7466=EDGE_CURVE('',#6030,#6030,#5122,.T.);
#7467=EDGE_CURVE('',#6030,#6019,#1497,.T.);
#7468=EDGE_CURVE('',#6031,#6031,#5123,.T.);
#7469=EDGE_CURVE('',#6031,#6020,#1498,.T.);
#7470=EDGE_CURVE('',#6032,#6032,#5124,.T.);
#7471=EDGE_CURVE('',#6032,#6021,#1499,.T.);
#7472=EDGE_CURVE('',#6033,#6033,#5125,.T.);
#7473=EDGE_CURVE('',#6033,#6022,#1500,.T.);
#7474=EDGE_CURVE('',#6034,#6034,#5126,.T.);
#7475=EDGE_CURVE('',#6034,#6023,#1501,.T.);
#7476=EDGE_CURVE('',#6035,#6035,#5127,.T.);
#7477=EDGE_CURVE('',#6035,#6024,#1502,.T.);
#7478=EDGE_CURVE('',#6036,#6036,#5128,.T.);
#7479=EDGE_CURVE('',#6036,#6025,#1503,.T.);
#7480=EDGE_CURVE('',#6037,#6037,#5129,.T.);
#7481=EDGE_CURVE('',#6037,#6026,#1504,.T.);
#7482=EDGE_CURVE('',#6038,#6038,#5130,.T.);
#7483=EDGE_CURVE('',#6038,#6027,#1505,.T.);
#7484=EDGE_CURVE('',#6015,#6039,#1506,.T.);
#7485=EDGE_CURVE('',#6040,#6039,#1507,.T.);
#7486=EDGE_CURVE('',#6016,#6040,#1508,.T.);
#7487=EDGE_CURVE('',#6011,#6041,#1509,.T.);
#7488=EDGE_CURVE('',#6042,#6041,#1510,.T.);
#7489=EDGE_CURVE('',#6012,#6042,#1511,.T.);
#7490=EDGE_CURVE('',#6043,#6042,#1512,.T.);
#7491=EDGE_CURVE('',#6013,#6043,#1513,.T.);
#7492=EDGE_CURVE('',#6044,#6043,#1514,.T.);
#7493=EDGE_CURVE('',#6014,#6044,#1515,.T.);
#7494=EDGE_CURVE('',#6039,#6044,#1516,.T.);
#7495=EDGE_CURVE('',#6045,#6046,#1517,.T.);
#7496=EDGE_CURVE('',#6045,#6040,#1518,.T.);
#7497=EDGE_CURVE('',#6041,#6046,#1519,.T.);
#7498=EDGE_CURVE('',#5988,#6047,#1520,.T.);
#7499=EDGE_CURVE('',#5991,#6048,#1521,.T.);
#7500=EDGE_CURVE('',#6047,#6048,#1522,.T.);
#7501=EDGE_CURVE('',#5970,#6045,#1523,.T.);
#7502=EDGE_CURVE('',#5967,#6046,#1524,.T.);
#7503=EDGE_CURVE('',#6049,#6047,#1525,.T.);
#7504=EDGE_CURVE('',#6010,#6049,#1526,.T.);
#7505=EDGE_CURVE('',#6050,#6049,#1527,.T.);
#7506=EDGE_CURVE('',#6009,#6050,#1528,.T.);
#7507=EDGE_CURVE('',#6048,#6050,#1529,.T.);
#7508=EDGE_CURVE('',#6051,#6052,#1530,.T.);
#7509=EDGE_CURVE('',#6053,#6051,#1531,.T.);
#7510=EDGE_CURVE('',#6054,#6053,#1532,.T.);
#7511=EDGE_CURVE('',#6055,#6054,#1533,.T.);
#7512=EDGE_CURVE('',#6056,#6055,#1534,.T.);
#7513=EDGE_CURVE('',#6052,#6056,#1535,.T.);
#7514=EDGE_CURVE('',#6057,#6057,#5131,.F.);
#7515=EDGE_CURVE('',#6051,#6058,#1536,.T.);
#7516=EDGE_CURVE('',#6059,#6058,#1537,.T.);
#7517=EDGE_CURVE('',#6053,#6059,#1538,.T.);
#7518=EDGE_CURVE('',#6060,#6059,#1539,.T.);
#7519=EDGE_CURVE('',#6054,#6060,#1540,.T.);
#7520=EDGE_CURVE('',#6061,#6060,#1541,.T.);
#7521=EDGE_CURVE('',#6055,#6061,#1542,.T.);
#7522=EDGE_CURVE('',#6062,#6061,#1543,.T.);
#7523=EDGE_CURVE('',#6056,#6062,#1544,.T.);
#7524=EDGE_CURVE('',#6063,#6062,#1545,.T.);
#7525=EDGE_CURVE('',#6052,#6063,#1546,.T.);
#7526=EDGE_CURVE('',#6058,#6063,#1547,.T.);
#7527=EDGE_CURVE('',#6064,#6064,#5132,.T.);
#7528=EDGE_CURVE('',#6064,#6057,#1548,.T.);
#7529=EDGE_CURVE('',#6065,#6065,#5133,.T.);
#7530=EDGE_CURVE('',#6065,#6066,#1549,.T.);
#7531=EDGE_CURVE('',#6066,#6066,#5134,.F.);
#7532=EDGE_CURVE('',#6067,#6068,#1550,.T.);
#7533=EDGE_CURVE('',#6067,#6069,#1551,.T.);
#7534=EDGE_CURVE('',#6070,#6069,#1552,.T.);
#7535=EDGE_CURVE('',#6068,#6070,#1553,.T.);
#7536=EDGE_CURVE('',#6068,#6071,#1554,.T.);
#7537=EDGE_CURVE('',#6072,#6070,#1555,.T.);
#7538=EDGE_CURVE('',#6071,#6072,#1556,.T.);
#7539=EDGE_CURVE('',#6071,#6073,#1557,.T.);
#7540=EDGE_CURVE('',#6074,#6072,#1558,.T.);
#7541=EDGE_CURVE('',#6073,#6074,#1559,.T.);
#7542=EDGE_CURVE('',#6073,#6075,#1560,.T.);
#7543=EDGE_CURVE('',#6076,#6074,#1561,.T.);
#7544=EDGE_CURVE('',#6075,#6076,#1562,.T.);
#7545=EDGE_CURVE('',#6075,#6077,#1563,.T.);
#7546=EDGE_CURVE('',#6078,#6076,#1564,.T.);
#7547=EDGE_CURVE('',#6077,#6078,#1565,.T.);
#7548=EDGE_CURVE('',#6077,#6067,#1566,.T.);
#7549=EDGE_CURVE('',#6069,#6078,#1567,.T.);
#7550=EDGE_CURVE('',#6079,#6079,#5135,.T.);
#7551=EDGE_CURVE('',#6079,#6080,#1568,.T.);
#7552=EDGE_CURVE('',#6080,#6080,#5136,.F.);
#7553=EDGE_CURVE('',#6081,#6082,#1569,.T.);
#7554=EDGE_CURVE('',#6081,#6083,#1570,.T.);
#7555=EDGE_CURVE('',#6084,#6083,#1571,.T.);
#7556=EDGE_CURVE('',#6082,#6084,#1572,.T.);
#7557=EDGE_CURVE('',#6082,#6085,#1573,.T.);
#7558=EDGE_CURVE('',#6086,#6084,#1574,.T.);
#7559=EDGE_CURVE('',#6085,#6086,#1575,.T.);
#7560=EDGE_CURVE('',#6085,#6087,#1576,.T.);
#7561=EDGE_CURVE('',#6088,#6086,#1577,.T.);
#7562=EDGE_CURVE('',#6087,#6088,#1578,.T.);
#7563=EDGE_CURVE('',#6087,#6089,#1579,.T.);
#7564=EDGE_CURVE('',#6090,#6088,#1580,.T.);
#7565=EDGE_CURVE('',#6089,#6090,#1581,.T.);
#7566=EDGE_CURVE('',#6089,#6091,#1582,.T.);
#7567=EDGE_CURVE('',#6092,#6090,#1583,.T.);
#7568=EDGE_CURVE('',#6091,#6092,#1584,.T.);
#7569=EDGE_CURVE('',#6091,#6081,#1585,.T.);
#7570=EDGE_CURVE('',#6083,#6092,#1586,.T.);
#7571=EDGE_CURVE('',#6093,#6094,#1587,.T.);
#7572=EDGE_CURVE('',#6094,#6095,#1588,.T.);
#7573=EDGE_CURVE('',#6095,#6096,#1589,.T.);
#7574=EDGE_CURVE('',#6093,#6096,#1590,.T.);
#7575=EDGE_CURVE('',#6097,#6094,#5137,.T.);
#7576=EDGE_CURVE('',#6097,#6098,#1591,.T.);
#7577=EDGE_CURVE('',#6098,#6095,#5138,.T.);
#7578=EDGE_CURVE('',#6097,#6099,#1592,.T.);
#7579=EDGE_CURVE('',#6100,#6099,#1593,.T.);
#7580=EDGE_CURVE('',#6100,#6098,#1594,.T.);
#7581=EDGE_CURVE('',#6101,#6102,#1595,.T.);
#7582=EDGE_CURVE('',#6101,#6103,#1596,.T.);
#7583=EDGE_CURVE('',#6103,#6104,#1597,.T.);
#7584=EDGE_CURVE('',#6102,#6104,#1598,.T.);
#7585=EDGE_CURVE('',#6101,#6105,#5139,.T.);
#7586=EDGE_CURVE('',#6105,#6106,#1599,.T.);
#7587=EDGE_CURVE('',#6106,#6103,#5140,.T.);
#7588=EDGE_CURVE('',#6107,#6105,#1600,.T.);
#7589=EDGE_CURVE('',#6107,#6108,#1601,.T.);
#7590=EDGE_CURVE('',#6108,#6106,#1602,.T.);
#7591=EDGE_CURVE('',#6109,#6107,#5141,.T.);
#7592=EDGE_CURVE('',#6109,#6110,#1603,.T.);
#7593=EDGE_CURVE('',#6110,#6108,#5142,.T.);
#7594=EDGE_CURVE('',#6111,#6093,#5143,.T.);
#7595=EDGE_CURVE('',#6096,#6112,#5144,.T.);
#7596=EDGE_CURVE('',#6111,#6112,#1604,.T.);
#7597=EDGE_CURVE('',#6109,#6113,#1605,.T.);
#7598=EDGE_CURVE('',#6113,#6114,#1606,.T.);
#7599=EDGE_CURVE('',#6114,#6110,#1607,.T.);
#7600=EDGE_CURVE('',#6115,#6116,#1608,.T.);
#7601=EDGE_CURVE('',#6115,#6117,#1609,.T.);
#7602=EDGE_CURVE('',#6118,#6117,#1610,.T.);
#7603=EDGE_CURVE('',#6116,#6118,#1611,.T.);
#7604=EDGE_CURVE('',#6119,#6116,#5145,.T.);
#7605=EDGE_CURVE('',#6120,#6118,#5146,.T.);
#7606=EDGE_CURVE('',#6119,#6120,#1612,.T.);
#7607=EDGE_CURVE('',#6119,#6121,#1613,.T.);
#7608=EDGE_CURVE('',#6122,#6120,#1614,.T.);
#7609=EDGE_CURVE('',#6121,#6122,#1615,.T.);
#7610=EDGE_CURVE('',#6123,#6124,#1616,.T.);
#7611=EDGE_CURVE('',#6125,#6124,#1617,.T.);
#7612=EDGE_CURVE('',#6126,#6125,#1618,.T.);
#7613=EDGE_CURVE('',#6123,#6126,#1619,.T.);
#7614=EDGE_CURVE('',#6123,#6127,#5147,.T.);
#7615=EDGE_CURVE('',#6128,#6126,#5148,.T.);
#7616=EDGE_CURVE('',#6127,#6128,#1620,.T.);
#7617=EDGE_CURVE('',#6129,#6127,#1621,.T.);
#7618=EDGE_CURVE('',#6130,#6128,#1622,.T.);
#7619=EDGE_CURVE('',#6129,#6130,#1623,.T.);
#7620=EDGE_CURVE('',#6113,#6129,#5149,.T.);
#7621=EDGE_CURVE('',#6114,#6130,#5150,.T.);
#7622=EDGE_CURVE('',#6131,#6112,#1624,.T.);
#7623=EDGE_CURVE('',#6132,#6131,#1625,.T.);
#7624=EDGE_CURVE('',#6111,#6132,#1626,.T.);
#7625=EDGE_CURVE('',#6132,#6115,#5151,.T.);
#7626=EDGE_CURVE('',#6117,#6131,#5152,.T.);
#7627=EDGE_CURVE('',#6133,#6122,#1627,.T.);
#7628=EDGE_CURVE('',#6134,#6133,#1628,.T.);
#7629=EDGE_CURVE('',#6134,#6121,#1629,.T.);
#7630=EDGE_CURVE('',#6099,#6135,#1630,.T.);
#7631=EDGE_CURVE('',#6135,#6136,#1631,.T.);
#7632=EDGE_CURVE('',#6100,#6136,#1632,.T.);
#7633=EDGE_CURVE('',#6125,#6104,#1633,.T.);
#7634=EDGE_CURVE('',#6124,#6102,#1634,.T.);
#7635=EDGE_CURVE('',#6137,#6135,#5153,.T.);
#7636=EDGE_CURVE('',#6137,#6138,#1635,.T.);
#7637=EDGE_CURVE('',#6138,#6136,#5154,.T.);
#7638=EDGE_CURVE('',#6137,#6139,#1636,.T.);
#7639=EDGE_CURVE('',#6139,#6140,#1637,.T.);
#7640=EDGE_CURVE('',#6140,#6138,#1638,.T.);
#7641=EDGE_CURVE('',#6141,#6139,#5155,.T.);
#7642=EDGE_CURVE('',#6141,#6142,#1639,.T.);
#7643=EDGE_CURVE('',#6142,#6140,#5156,.T.);
#7644=EDGE_CURVE('',#6141,#6143,#1640,.T.);
#7645=EDGE_CURVE('',#6143,#6144,#1641,.T.);
#7646=EDGE_CURVE('',#6144,#6142,#1642,.T.);
#7647=EDGE_CURVE('',#6145,#6143,#1643,.T.);
#7648=EDGE_CURVE('',#6145,#6146,#1644,.T.);
#7649=EDGE_CURVE('',#6146,#6144,#1645,.T.);
#7650=EDGE_CURVE('',#6147,#6145,#1646,.T.);
#7651=EDGE_CURVE('',#6147,#6148,#1647,.T.);
#7652=EDGE_CURVE('',#6148,#6146,#1648,.T.);
#7653=EDGE_CURVE('',#6147,#6149,#5157,.T.);
#7654=EDGE_CURVE('',#6149,#6150,#1649,.T.);
#7655=EDGE_CURVE('',#6150,#6148,#5158,.T.);
#7656=EDGE_CURVE('',#6151,#6149,#1650,.T.);
#7657=EDGE_CURVE('',#6151,#6152,#1651,.T.);
#7658=EDGE_CURVE('',#6152,#6150,#1652,.T.);
#7659=EDGE_CURVE('',#6151,#6153,#5159,.T.);
#7660=EDGE_CURVE('',#6153,#6154,#1653,.T.);
#7661=EDGE_CURVE('',#6154,#6152,#5160,.T.);
#7662=EDGE_CURVE('',#6153,#6155,#1654,.T.);
#7663=EDGE_CURVE('',#6155,#6156,#1655,.T.);
#7664=EDGE_CURVE('',#6156,#6154,#1656,.T.);
#7665=EDGE_CURVE('',#6157,#6134,#5161,.T.);
#7666=EDGE_CURVE('',#6158,#6133,#5162,.T.);
#7667=EDGE_CURVE('',#6157,#6158,#1657,.T.);
#7668=EDGE_CURVE('',#6157,#6159,#1658,.T.);
#7669=EDGE_CURVE('',#6160,#6158,#1659,.T.);
#7670=EDGE_CURVE('',#6159,#6160,#1660,.T.);
#7671=EDGE_CURVE('',#6161,#6159,#5163,.T.);
#7672=EDGE_CURVE('',#6162,#6160,#5164,.T.);
#7673=EDGE_CURVE('',#6161,#6162,#1661,.T.);
#7674=EDGE_CURVE('',#6161,#6163,#1662,.T.);
#7675=EDGE_CURVE('',#6164,#6162,#1663,.T.);
#7676=EDGE_CURVE('',#6163,#6164,#1664,.T.);
#7677=EDGE_CURVE('',#6165,#6163,#1665,.T.);
#7678=EDGE_CURVE('',#6166,#6164,#1666,.T.);
#7679=EDGE_CURVE('',#6165,#6166,#1667,.T.);
#7680=EDGE_CURVE('',#6167,#6165,#1668,.T.);
#7681=EDGE_CURVE('',#6168,#6166,#1669,.T.);
#7682=EDGE_CURVE('',#6167,#6168,#1670,.T.);
#7683=EDGE_CURVE('',#6167,#6169,#5165,.T.);
#7684=EDGE_CURVE('',#6170,#6168,#5166,.T.);
#7685=EDGE_CURVE('',#6169,#6170,#1671,.T.);
#7686=EDGE_CURVE('',#6171,#6169,#1672,.T.);
#7687=EDGE_CURVE('',#6172,#6170,#1673,.T.);
#7688=EDGE_CURVE('',#6171,#6172,#1674,.T.);
#7689=EDGE_CURVE('',#6171,#6155,#5167,.T.);
#7690=EDGE_CURVE('',#6156,#6172,#5168,.T.);
#7691=EDGE_CURVE('',#6173,#6173,#5169,.T.);
#7692=EDGE_CURVE('',#6173,#6174,#1675,.T.);
#7693=EDGE_CURVE('',#6174,#6174,#5170,.F.);
#7694=EDGE_CURVE('',#6175,#6176,#1676,.T.);
#7695=EDGE_CURVE('',#6175,#6177,#1677,.T.);
#7696=EDGE_CURVE('',#6178,#6177,#1678,.T.);
#7697=EDGE_CURVE('',#6176,#6178,#1679,.T.);
#7698=EDGE_CURVE('',#6176,#6179,#1680,.T.);
#7699=EDGE_CURVE('',#6180,#6178,#1681,.T.);
#7700=EDGE_CURVE('',#6179,#6180,#1682,.T.);
#7701=EDGE_CURVE('',#6179,#6181,#1683,.T.);
#7702=EDGE_CURVE('',#6182,#6180,#1684,.T.);
#7703=EDGE_CURVE('',#6181,#6182,#1685,.T.);
#7704=EDGE_CURVE('',#6181,#6183,#1686,.T.);
#7705=EDGE_CURVE('',#6184,#6182,#1687,.T.);
#7706=EDGE_CURVE('',#6183,#6184,#1688,.T.);
#7707=EDGE_CURVE('',#6183,#6185,#1689,.T.);
#7708=EDGE_CURVE('',#6186,#6184,#1690,.T.);
#7709=EDGE_CURVE('',#6185,#6186,#1691,.T.);
#7710=EDGE_CURVE('',#6185,#6175,#1692,.T.);
#7711=EDGE_CURVE('',#6177,#6186,#1693,.T.);
#7712=ORIENTED_EDGE('',*,*,#6187,.T.);
#7713=ORIENTED_EDGE('',*,*,#6188,.T.);
#7714=ORIENTED_EDGE('',*,*,#6189,.T.);
#7715=ORIENTED_EDGE('',*,*,#6190,.T.);
#7716=ORIENTED_EDGE('',*,*,#6188,.F.);
#7717=ORIENTED_EDGE('',*,*,#6190,.F.);
#7718=ORIENTED_EDGE('',*,*,#6191,.T.);
#7719=ORIENTED_EDGE('',*,*,#6192,.F.);
#7720=ORIENTED_EDGE('',*,*,#6193,.F.);
#7721=ORIENTED_EDGE('',*,*,#6191,.F.);
#7722=ORIENTED_EDGE('',*,*,#6189,.F.);
#7723=ORIENTED_EDGE('',*,*,#6187,.F.);
#7724=ORIENTED_EDGE('',*,*,#6193,.T.);
#7725=ORIENTED_EDGE('',*,*,#6194,.T.);
#7726=ORIENTED_EDGE('',*,*,#6195,.F.);
#7727=ORIENTED_EDGE('',*,*,#6194,.F.);
#7728=ORIENTED_EDGE('',*,*,#6192,.T.);
#7729=ORIENTED_EDGE('',*,*,#6196,.T.);
#7730=ORIENTED_EDGE('',*,*,#6197,.T.);
#7731=ORIENTED_EDGE('',*,*,#6198,.F.);
#7732=ORIENTED_EDGE('',*,*,#6197,.F.);
#7733=ORIENTED_EDGE('',*,*,#6199,.T.);
#7734=ORIENTED_EDGE('',*,*,#6200,.F.);
#7735=ORIENTED_EDGE('',*,*,#6201,.T.);
#7736=ORIENTED_EDGE('',*,*,#6199,.F.);
#7737=ORIENTED_EDGE('',*,*,#6196,.F.);
#7738=ORIENTED_EDGE('',*,*,#6201,.F.);
#7739=ORIENTED_EDGE('',*,*,#6202,.F.);
#7740=ORIENTED_EDGE('',*,*,#6195,.T.);
#7741=ORIENTED_EDGE('',*,*,#6203,.T.);
#7742=ORIENTED_EDGE('',*,*,#6202,.T.);
#7743=ORIENTED_EDGE('',*,*,#6200,.T.);
#7744=ORIENTED_EDGE('',*,*,#6203,.F.);
#7745=ORIENTED_EDGE('',*,*,#6204,.F.);
#7746=ORIENTED_EDGE('',*,*,#6204,.T.);
#7747=ORIENTED_EDGE('',*,*,#6205,.T.);
#7748=ORIENTED_EDGE('',*,*,#6206,.F.);
#7749=ORIENTED_EDGE('',*,*,#6205,.F.);
#7750=ORIENTED_EDGE('',*,*,#6207,.T.);
#7751=ORIENTED_EDGE('',*,*,#6208,.T.);
#7752=ORIENTED_EDGE('',*,*,#6209,.T.);
#7753=ORIENTED_EDGE('',*,*,#6210,.T.);
#7754=ORIENTED_EDGE('',*,*,#6208,.F.);
#7755=ORIENTED_EDGE('',*,*,#6210,.F.);
#7756=ORIENTED_EDGE('',*,*,#6211,.T.);
#7757=ORIENTED_EDGE('',*,*,#6212,.F.);
#7758=ORIENTED_EDGE('',*,*,#6213,.F.);
#7759=ORIENTED_EDGE('',*,*,#6211,.F.);
#7760=ORIENTED_EDGE('',*,*,#6209,.F.);
#7761=ORIENTED_EDGE('',*,*,#6207,.F.);
#7762=ORIENTED_EDGE('',*,*,#6206,.T.);
#7763=ORIENTED_EDGE('',*,*,#6198,.T.);
#7764=ORIENTED_EDGE('',*,*,#6214,.T.);
#7765=ORIENTED_EDGE('',*,*,#6212,.T.);
#7766=ORIENTED_EDGE('',*,*,#6213,.T.);
#7767=ORIENTED_EDGE('',*,*,#6214,.F.);
#7768=ORIENTED_EDGE('',*,*,#6215,.T.);
#7769=ORIENTED_EDGE('',*,*,#6216,.F.);
#7770=ORIENTED_EDGE('',*,*,#6215,.F.);
#7771=ORIENTED_EDGE('',*,*,#6217,.T.);
#7772=ORIENTED_EDGE('',*,*,#6218,.T.);
#7773=ORIENTED_EDGE('',*,*,#6217,.F.);
#7774=ORIENTED_EDGE('',*,*,#6218,.F.);
#7775=ORIENTED_EDGE('',*,*,#6219,.T.);
#7776=ORIENTED_EDGE('',*,*,#6220,.T.);
#7777=ORIENTED_EDGE('',*,*,#6221,.F.);
#7778=ORIENTED_EDGE('',*,*,#6222,.F.);
#7779=ORIENTED_EDGE('',*,*,#6223,.F.);
#7780=ORIENTED_EDGE('',*,*,#6220,.F.);
#7781=ORIENTED_EDGE('',*,*,#6224,.T.);
#7782=ORIENTED_EDGE('',*,*,#6222,.T.);
#7783=ORIENTED_EDGE('',*,*,#6224,.F.);
#7784=ORIENTED_EDGE('',*,*,#6216,.T.);
#7785=ORIENTED_EDGE('',*,*,#6225,.T.);
#7786=ORIENTED_EDGE('',*,*,#6223,.T.);
#7787=ORIENTED_EDGE('',*,*,#6225,.F.);
#7788=ORIENTED_EDGE('',*,*,#6226,.F.);
#7789=ORIENTED_EDGE('',*,*,#6227,.T.);
#7790=ORIENTED_EDGE('',*,*,#6228,.F.);
#7791=ORIENTED_EDGE('',*,*,#6229,.T.);
#7792=ORIENTED_EDGE('',*,*,#6226,.T.);
#7793=ORIENTED_EDGE('',*,*,#6229,.F.);
#7794=ORIENTED_EDGE('',*,*,#6228,.T.);
#7795=ORIENTED_EDGE('',*,*,#6230,.T.);
#7796=ORIENTED_EDGE('',*,*,#6219,.F.);
#7797=ORIENTED_EDGE('',*,*,#6231,.T.);
#7798=ORIENTED_EDGE('',*,*,#6232,.F.);
#7799=ORIENTED_EDGE('',*,*,#6231,.F.);
#7800=ORIENTED_EDGE('',*,*,#6233,.T.);
#7801=ORIENTED_EDGE('',*,*,#6234,.T.);
#7802=ORIENTED_EDGE('',*,*,#6230,.F.);
#7803=ORIENTED_EDGE('',*,*,#6234,.F.);
#7804=ORIENTED_EDGE('',*,*,#6221,.T.);
#7805=ORIENTED_EDGE('',*,*,#6235,.T.);
#7806=ORIENTED_EDGE('',*,*,#6227,.F.);
#7807=ORIENTED_EDGE('',*,*,#6235,.F.);
#7808=ORIENTED_EDGE('',*,*,#6233,.F.);
#7809=ORIENTED_EDGE('',*,*,#6236,.F.);
#7810=ORIENTED_EDGE('',*,*,#6237,.F.);
#7811=ORIENTED_EDGE('',*,*,#6238,.T.);
#7812=ORIENTED_EDGE('',*,*,#6236,.T.);
#7813=ORIENTED_EDGE('',*,*,#6238,.F.);
#7814=ORIENTED_EDGE('',*,*,#6232,.T.);
#7815=ORIENTED_EDGE('',*,*,#6237,.T.);
#7816=ORIENTED_EDGE('',*,*,#6239,.T.);
#7817=ORIENTED_EDGE('',*,*,#6240,.T.);
#7818=ORIENTED_EDGE('',*,*,#6241,.T.);
#7819=ORIENTED_EDGE('',*,*,#6242,.T.);
#7820=ORIENTED_EDGE('',*,*,#6242,.F.);
#7821=ORIENTED_EDGE('',*,*,#6243,.F.);
#7822=ORIENTED_EDGE('',*,*,#6244,.F.);
#7823=ORIENTED_EDGE('',*,*,#6245,.F.);
#7824=ORIENTED_EDGE('',*,*,#6246,.T.);
#7825=ORIENTED_EDGE('',*,*,#6247,.T.);
#7826=ORIENTED_EDGE('',*,*,#6248,.T.);
#7827=ORIENTED_EDGE('',*,*,#6249,.T.);
#7828=ORIENTED_EDGE('',*,*,#6250,.T.);
#7829=ORIENTED_EDGE('',*,*,#6251,.T.);
#7830=ORIENTED_EDGE('',*,*,#6252,.T.);
#7831=ORIENTED_EDGE('',*,*,#6253,.T.);
#7832=ORIENTED_EDGE('',*,*,#6254,.T.);
#7833=ORIENTED_EDGE('',*,*,#6255,.T.);
#7834=ORIENTED_EDGE('',*,*,#6256,.T.);
#7835=ORIENTED_EDGE('',*,*,#6241,.F.);
#7836=ORIENTED_EDGE('',*,*,#6257,.T.);
#7837=ORIENTED_EDGE('',*,*,#6258,.T.);
#7838=ORIENTED_EDGE('',*,*,#6259,.F.);
#7839=ORIENTED_EDGE('',*,*,#6260,.F.);
#7840=ORIENTED_EDGE('',*,*,#6261,.F.);
#7841=ORIENTED_EDGE('',*,*,#6262,.T.);
#7842=ORIENTED_EDGE('',*,*,#6263,.T.);
#7843=ORIENTED_EDGE('',*,*,#6264,.F.);
#7844=ORIENTED_EDGE('',*,*,#6243,.T.);
#7845=ORIENTED_EDGE('',*,*,#6265,.T.);
#7846=ORIENTED_EDGE('',*,*,#6244,.T.);
#7847=ORIENTED_EDGE('',*,*,#6264,.T.);
#7848=ORIENTED_EDGE('',*,*,#6266,.T.);
#7849=ORIENTED_EDGE('',*,*,#6267,.F.);
#7850=ORIENTED_EDGE('',*,*,#6268,.T.);
#7851=ORIENTED_EDGE('',*,*,#6269,.F.);
#7852=ORIENTED_EDGE('',*,*,#6268,.F.);
#7853=ORIENTED_EDGE('',*,*,#6270,.F.);
#7854=ORIENTED_EDGE('',*,*,#6271,.T.);
#7855=ORIENTED_EDGE('',*,*,#6272,.F.);
#7856=ORIENTED_EDGE('',*,*,#6271,.F.);
#7857=ORIENTED_EDGE('',*,*,#6273,.F.);
#7858=ORIENTED_EDGE('',*,*,#6274,.T.);
#7859=ORIENTED_EDGE('',*,*,#6275,.F.);
#7860=ORIENTED_EDGE('',*,*,#6274,.F.);
#7861=ORIENTED_EDGE('',*,*,#6276,.F.);
#7862=ORIENTED_EDGE('',*,*,#6277,.T.);
#7863=ORIENTED_EDGE('',*,*,#6278,.F.);
#7864=ORIENTED_EDGE('',*,*,#6277,.F.);
#7865=ORIENTED_EDGE('',*,*,#6279,.F.);
#7866=ORIENTED_EDGE('',*,*,#6280,.T.);
#7867=ORIENTED_EDGE('',*,*,#6281,.F.);
#7868=ORIENTED_EDGE('',*,*,#6280,.F.);
#7869=ORIENTED_EDGE('',*,*,#6282,.F.);
#7870=ORIENTED_EDGE('',*,*,#6283,.T.);
#7871=ORIENTED_EDGE('',*,*,#6284,.F.);
#7872=ORIENTED_EDGE('',*,*,#6283,.F.);
#7873=ORIENTED_EDGE('',*,*,#6285,.F.);
#7874=ORIENTED_EDGE('',*,*,#6286,.T.);
#7875=ORIENTED_EDGE('',*,*,#6287,.F.);
#7876=ORIENTED_EDGE('',*,*,#6286,.F.);
#7877=ORIENTED_EDGE('',*,*,#6288,.F.);
#7878=ORIENTED_EDGE('',*,*,#6289,.T.);
#7879=ORIENTED_EDGE('',*,*,#6290,.F.);
#7880=ORIENTED_EDGE('',*,*,#6289,.F.);
#7881=ORIENTED_EDGE('',*,*,#6291,.F.);
#7882=ORIENTED_EDGE('',*,*,#6292,.T.);
#7883=ORIENTED_EDGE('',*,*,#6293,.F.);
#7884=ORIENTED_EDGE('',*,*,#6292,.F.);
#7885=ORIENTED_EDGE('',*,*,#6294,.F.);
#7886=ORIENTED_EDGE('',*,*,#6295,.T.);
#7887=ORIENTED_EDGE('',*,*,#6296,.F.);
#7888=ORIENTED_EDGE('',*,*,#6295,.F.);
#7889=ORIENTED_EDGE('',*,*,#6297,.F.);
#7890=ORIENTED_EDGE('',*,*,#6298,.T.);
#7891=ORIENTED_EDGE('',*,*,#6299,.F.);
#7892=ORIENTED_EDGE('',*,*,#6298,.F.);
#7893=ORIENTED_EDGE('',*,*,#6256,.F.);
#7894=ORIENTED_EDGE('',*,*,#6300,.T.);
#7895=ORIENTED_EDGE('',*,*,#6301,.F.);
#7896=ORIENTED_EDGE('',*,*,#6300,.F.);
#7897=ORIENTED_EDGE('',*,*,#6255,.F.);
#7898=ORIENTED_EDGE('',*,*,#6302,.T.);
#7899=ORIENTED_EDGE('',*,*,#6303,.F.);
#7900=ORIENTED_EDGE('',*,*,#6302,.F.);
#7901=ORIENTED_EDGE('',*,*,#6254,.F.);
#7902=ORIENTED_EDGE('',*,*,#6304,.T.);
#7903=ORIENTED_EDGE('',*,*,#6305,.F.);
#7904=ORIENTED_EDGE('',*,*,#6304,.F.);
#7905=ORIENTED_EDGE('',*,*,#6253,.F.);
#7906=ORIENTED_EDGE('',*,*,#6306,.T.);
#7907=ORIENTED_EDGE('',*,*,#6307,.F.);
#7908=ORIENTED_EDGE('',*,*,#6306,.F.);
#7909=ORIENTED_EDGE('',*,*,#6252,.F.);
#7910=ORIENTED_EDGE('',*,*,#6308,.T.);
#7911=ORIENTED_EDGE('',*,*,#6309,.F.);
#7912=ORIENTED_EDGE('',*,*,#6308,.F.);
#7913=ORIENTED_EDGE('',*,*,#6251,.F.);
#7914=ORIENTED_EDGE('',*,*,#6310,.T.);
#7915=ORIENTED_EDGE('',*,*,#6311,.F.);
#7916=ORIENTED_EDGE('',*,*,#6310,.F.);
#7917=ORIENTED_EDGE('',*,*,#6250,.F.);
#7918=ORIENTED_EDGE('',*,*,#6312,.T.);
#7919=ORIENTED_EDGE('',*,*,#6313,.F.);
#7920=ORIENTED_EDGE('',*,*,#6312,.F.);
#7921=ORIENTED_EDGE('',*,*,#6249,.F.);
#7922=ORIENTED_EDGE('',*,*,#6314,.T.);
#7923=ORIENTED_EDGE('',*,*,#6315,.F.);
#7924=ORIENTED_EDGE('',*,*,#6314,.F.);
#7925=ORIENTED_EDGE('',*,*,#6248,.F.);
#7926=ORIENTED_EDGE('',*,*,#6316,.T.);
#7927=ORIENTED_EDGE('',*,*,#6317,.F.);
#7928=ORIENTED_EDGE('',*,*,#6316,.F.);
#7929=ORIENTED_EDGE('',*,*,#6247,.F.);
#7930=ORIENTED_EDGE('',*,*,#6318,.T.);
#7931=ORIENTED_EDGE('',*,*,#6319,.F.);
#7932=ORIENTED_EDGE('',*,*,#6318,.F.);
#7933=ORIENTED_EDGE('',*,*,#6246,.F.);
#7934=ORIENTED_EDGE('',*,*,#6320,.T.);
#7935=ORIENTED_EDGE('',*,*,#6321,.F.);
#7936=ORIENTED_EDGE('',*,*,#6320,.F.);
#7937=ORIENTED_EDGE('',*,*,#6322,.F.);
#7938=ORIENTED_EDGE('',*,*,#6323,.T.);
#7939=ORIENTED_EDGE('',*,*,#6324,.F.);
#7940=ORIENTED_EDGE('',*,*,#6323,.F.);
#7941=ORIENTED_EDGE('',*,*,#6325,.F.);
#7942=ORIENTED_EDGE('',*,*,#6326,.T.);
#7943=ORIENTED_EDGE('',*,*,#6327,.F.);
#7944=ORIENTED_EDGE('',*,*,#6326,.F.);
#7945=ORIENTED_EDGE('',*,*,#6328,.F.);
#7946=ORIENTED_EDGE('',*,*,#6329,.T.);
#7947=ORIENTED_EDGE('',*,*,#6330,.F.);
#7948=ORIENTED_EDGE('',*,*,#6329,.F.);
#7949=ORIENTED_EDGE('',*,*,#6331,.F.);
#7950=ORIENTED_EDGE('',*,*,#6332,.T.);
#7951=ORIENTED_EDGE('',*,*,#6333,.F.);
#7952=ORIENTED_EDGE('',*,*,#6332,.F.);
#7953=ORIENTED_EDGE('',*,*,#6334,.F.);
#7954=ORIENTED_EDGE('',*,*,#6335,.T.);
#7955=ORIENTED_EDGE('',*,*,#6336,.F.);
#7956=ORIENTED_EDGE('',*,*,#6335,.F.);
#7957=ORIENTED_EDGE('',*,*,#6337,.F.);
#7958=ORIENTED_EDGE('',*,*,#6338,.T.);
#7959=ORIENTED_EDGE('',*,*,#6339,.F.);
#7960=ORIENTED_EDGE('',*,*,#6338,.F.);
#7961=ORIENTED_EDGE('',*,*,#6340,.F.);
#7962=ORIENTED_EDGE('',*,*,#6341,.T.);
#7963=ORIENTED_EDGE('',*,*,#6342,.F.);
#7964=ORIENTED_EDGE('',*,*,#6341,.F.);
#7965=ORIENTED_EDGE('',*,*,#6343,.F.);
#7966=ORIENTED_EDGE('',*,*,#6344,.T.);
#7967=ORIENTED_EDGE('',*,*,#6345,.F.);
#7968=ORIENTED_EDGE('',*,*,#6344,.F.);
#7969=ORIENTED_EDGE('',*,*,#6346,.F.);
#7970=ORIENTED_EDGE('',*,*,#6347,.T.);
#7971=ORIENTED_EDGE('',*,*,#6348,.F.);
#7972=ORIENTED_EDGE('',*,*,#6347,.F.);
#7973=ORIENTED_EDGE('',*,*,#6349,.F.);
#7974=ORIENTED_EDGE('',*,*,#6350,.T.);
#7975=ORIENTED_EDGE('',*,*,#6351,.F.);
#7976=ORIENTED_EDGE('',*,*,#6350,.F.);
#7977=ORIENTED_EDGE('',*,*,#6352,.F.);
#7978=ORIENTED_EDGE('',*,*,#6353,.T.);
#7979=ORIENTED_EDGE('',*,*,#6354,.F.);
#7980=ORIENTED_EDGE('',*,*,#6353,.F.);
#7981=ORIENTED_EDGE('',*,*,#6262,.F.);
#7982=ORIENTED_EDGE('',*,*,#6355,.T.);
#7983=ORIENTED_EDGE('',*,*,#6356,.F.);
#7984=ORIENTED_EDGE('',*,*,#6357,.F.);
#7985=ORIENTED_EDGE('',*,*,#6266,.F.);
#7986=ORIENTED_EDGE('',*,*,#6263,.F.);
#7987=ORIENTED_EDGE('',*,*,#6357,.T.);
#7988=ORIENTED_EDGE('',*,*,#6358,.F.);
#7989=ORIENTED_EDGE('',*,*,#6352,.T.);
#7990=ORIENTED_EDGE('',*,*,#6349,.T.);
#7991=ORIENTED_EDGE('',*,*,#6346,.T.);
#7992=ORIENTED_EDGE('',*,*,#6343,.T.);
#7993=ORIENTED_EDGE('',*,*,#6340,.T.);
#7994=ORIENTED_EDGE('',*,*,#6337,.T.);
#7995=ORIENTED_EDGE('',*,*,#6334,.T.);
#7996=ORIENTED_EDGE('',*,*,#6331,.T.);
#7997=ORIENTED_EDGE('',*,*,#6328,.T.);
#7998=ORIENTED_EDGE('',*,*,#6325,.T.);
#7999=ORIENTED_EDGE('',*,*,#6322,.T.);
#8000=ORIENTED_EDGE('',*,*,#6240,.F.);
#8001=ORIENTED_EDGE('',*,*,#6359,.F.);
#8002=ORIENTED_EDGE('',*,*,#6360,.F.);
#8003=ORIENTED_EDGE('',*,*,#6257,.F.);
#8004=ORIENTED_EDGE('',*,*,#6299,.T.);
#8005=ORIENTED_EDGE('',*,*,#6296,.T.);
#8006=ORIENTED_EDGE('',*,*,#6293,.T.);
#8007=ORIENTED_EDGE('',*,*,#6290,.T.);
#8008=ORIENTED_EDGE('',*,*,#6287,.T.);
#8009=ORIENTED_EDGE('',*,*,#6284,.T.);
#8010=ORIENTED_EDGE('',*,*,#6281,.T.);
#8011=ORIENTED_EDGE('',*,*,#6278,.T.);
#8012=ORIENTED_EDGE('',*,*,#6275,.T.);
#8013=ORIENTED_EDGE('',*,*,#6272,.T.);
#8014=ORIENTED_EDGE('',*,*,#6269,.T.);
#8015=ORIENTED_EDGE('',*,*,#6258,.F.);
#8016=ORIENTED_EDGE('',*,*,#6360,.T.);
#8017=ORIENTED_EDGE('',*,*,#6361,.F.);
#8018=ORIENTED_EDGE('',*,*,#6362,.F.);
#8019=ORIENTED_EDGE('',*,*,#6259,.T.);
#8020=ORIENTED_EDGE('',*,*,#6362,.T.);
#8021=ORIENTED_EDGE('',*,*,#6363,.F.);
#8022=ORIENTED_EDGE('',*,*,#6364,.F.);
#8023=ORIENTED_EDGE('',*,*,#6297,.T.);
#8024=ORIENTED_EDGE('',*,*,#6294,.T.);
#8025=ORIENTED_EDGE('',*,*,#6291,.T.);
#8026=ORIENTED_EDGE('',*,*,#6288,.T.);
#8027=ORIENTED_EDGE('',*,*,#6285,.T.);
#8028=ORIENTED_EDGE('',*,*,#6282,.T.);
#8029=ORIENTED_EDGE('',*,*,#6279,.T.);
#8030=ORIENTED_EDGE('',*,*,#6276,.T.);
#8031=ORIENTED_EDGE('',*,*,#6273,.T.);
#8032=ORIENTED_EDGE('',*,*,#6270,.T.);
#8033=ORIENTED_EDGE('',*,*,#6267,.T.);
#8034=ORIENTED_EDGE('',*,*,#6260,.T.);
#8035=ORIENTED_EDGE('',*,*,#6364,.T.);
#8036=ORIENTED_EDGE('',*,*,#6365,.F.);
#8037=ORIENTED_EDGE('',*,*,#6366,.F.);
#8038=ORIENTED_EDGE('',*,*,#6321,.T.);
#8039=ORIENTED_EDGE('',*,*,#6319,.T.);
#8040=ORIENTED_EDGE('',*,*,#6317,.T.);
#8041=ORIENTED_EDGE('',*,*,#6315,.T.);
#8042=ORIENTED_EDGE('',*,*,#6313,.T.);
#8043=ORIENTED_EDGE('',*,*,#6311,.T.);
#8044=ORIENTED_EDGE('',*,*,#6309,.T.);
#8045=ORIENTED_EDGE('',*,*,#6307,.T.);
#8046=ORIENTED_EDGE('',*,*,#6305,.T.);
#8047=ORIENTED_EDGE('',*,*,#6303,.T.);
#8048=ORIENTED_EDGE('',*,*,#6301,.T.);
#8049=ORIENTED_EDGE('',*,*,#6261,.T.);
#8050=ORIENTED_EDGE('',*,*,#6366,.T.);
#8051=ORIENTED_EDGE('',*,*,#6367,.F.);
#8052=ORIENTED_EDGE('',*,*,#6355,.F.);
#8053=ORIENTED_EDGE('',*,*,#6354,.T.);
#8054=ORIENTED_EDGE('',*,*,#6351,.T.);
#8055=ORIENTED_EDGE('',*,*,#6348,.T.);
#8056=ORIENTED_EDGE('',*,*,#6345,.T.);
#8057=ORIENTED_EDGE('',*,*,#6342,.T.);
#8058=ORIENTED_EDGE('',*,*,#6339,.T.);
#8059=ORIENTED_EDGE('',*,*,#6336,.T.);
#8060=ORIENTED_EDGE('',*,*,#6333,.T.);
#8061=ORIENTED_EDGE('',*,*,#6330,.T.);
#8062=ORIENTED_EDGE('',*,*,#6327,.T.);
#8063=ORIENTED_EDGE('',*,*,#6324,.T.);
#8064=ORIENTED_EDGE('',*,*,#6239,.F.);
#8065=ORIENTED_EDGE('',*,*,#6245,.T.);
#8066=ORIENTED_EDGE('',*,*,#6265,.F.);
#8067=ORIENTED_EDGE('',*,*,#6358,.T.);
#8068=ORIENTED_EDGE('',*,*,#6356,.T.);
#8069=ORIENTED_EDGE('',*,*,#6367,.T.);
#8070=ORIENTED_EDGE('',*,*,#6365,.T.);
#8071=ORIENTED_EDGE('',*,*,#6363,.T.);
#8072=ORIENTED_EDGE('',*,*,#6361,.T.);
#8073=ORIENTED_EDGE('',*,*,#6359,.T.);
#8074=ORIENTED_EDGE('',*,*,#6368,.F.);
#8075=ORIENTED_EDGE('',*,*,#6369,.F.);
#8076=ORIENTED_EDGE('',*,*,#6370,.F.);
#8077=ORIENTED_EDGE('',*,*,#6371,.F.);
#8078=ORIENTED_EDGE('',*,*,#6372,.F.);
#8079=ORIENTED_EDGE('',*,*,#6373,.F.);
#8080=ORIENTED_EDGE('',*,*,#6374,.T.);
#8081=ORIENTED_EDGE('',*,*,#6369,.T.);
#8082=ORIENTED_EDGE('',*,*,#6375,.T.);
#8083=ORIENTED_EDGE('',*,*,#6376,.F.);
#8084=ORIENTED_EDGE('',*,*,#6377,.F.);
#8085=ORIENTED_EDGE('',*,*,#6370,.T.);
#8086=ORIENTED_EDGE('',*,*,#6377,.T.);
#8087=ORIENTED_EDGE('',*,*,#6378,.F.);
#8088=ORIENTED_EDGE('',*,*,#6379,.F.);
#8089=ORIENTED_EDGE('',*,*,#6371,.T.);
#8090=ORIENTED_EDGE('',*,*,#6379,.T.);
#8091=ORIENTED_EDGE('',*,*,#6380,.F.);
#8092=ORIENTED_EDGE('',*,*,#6381,.F.);
#8093=ORIENTED_EDGE('',*,*,#6372,.T.);
#8094=ORIENTED_EDGE('',*,*,#6381,.T.);
#8095=ORIENTED_EDGE('',*,*,#6382,.F.);
#8096=ORIENTED_EDGE('',*,*,#6383,.F.);
#8097=ORIENTED_EDGE('',*,*,#6373,.T.);
#8098=ORIENTED_EDGE('',*,*,#6383,.T.);
#8099=ORIENTED_EDGE('',*,*,#6384,.F.);
#8100=ORIENTED_EDGE('',*,*,#6385,.F.);
#8101=ORIENTED_EDGE('',*,*,#6368,.T.);
#8102=ORIENTED_EDGE('',*,*,#6385,.T.);
#8103=ORIENTED_EDGE('',*,*,#6386,.F.);
#8104=ORIENTED_EDGE('',*,*,#6375,.F.);
#8105=ORIENTED_EDGE('',*,*,#6386,.T.);
#8106=ORIENTED_EDGE('',*,*,#6384,.T.);
#8107=ORIENTED_EDGE('',*,*,#6382,.T.);
#8108=ORIENTED_EDGE('',*,*,#6380,.T.);
#8109=ORIENTED_EDGE('',*,*,#6378,.T.);
#8110=ORIENTED_EDGE('',*,*,#6376,.T.);
#8111=ORIENTED_EDGE('',*,*,#6387,.F.);
#8112=ORIENTED_EDGE('',*,*,#6388,.T.);
#8113=ORIENTED_EDGE('',*,*,#6374,.F.);
#8114=ORIENTED_EDGE('',*,*,#6388,.F.);
#8115=ORIENTED_EDGE('',*,*,#6387,.T.);
#8116=ORIENTED_EDGE('',*,*,#6389,.T.);
#8117=ORIENTED_EDGE('',*,*,#6390,.T.);
#8118=ORIENTED_EDGE('',*,*,#6391,.T.);
#8119=ORIENTED_EDGE('',*,*,#6392,.F.);
#8120=ORIENTED_EDGE('',*,*,#6393,.F.);
#8121=ORIENTED_EDGE('',*,*,#6394,.T.);
#8122=ORIENTED_EDGE('',*,*,#6395,.T.);
#8123=ORIENTED_EDGE('',*,*,#6390,.F.);
#8124=ORIENTED_EDGE('',*,*,#6396,.T.);
#8125=ORIENTED_EDGE('',*,*,#6397,.F.);
#8126=ORIENTED_EDGE('',*,*,#6398,.T.);
#8127=ORIENTED_EDGE('',*,*,#6394,.F.);
#8128=ORIENTED_EDGE('',*,*,#6399,.F.);
#8129=ORIENTED_EDGE('',*,*,#6400,.T.);
#8130=ORIENTED_EDGE('',*,*,#6401,.T.);
#8131=ORIENTED_EDGE('',*,*,#6402,.F.);
#8132=ORIENTED_EDGE('',*,*,#6403,.T.);
#8133=ORIENTED_EDGE('',*,*,#6404,.T.);
#8134=ORIENTED_EDGE('',*,*,#6405,.T.);
#8135=ORIENTED_EDGE('',*,*,#6400,.F.);
#8136=ORIENTED_EDGE('',*,*,#6406,.F.);
#8137=ORIENTED_EDGE('',*,*,#6407,.T.);
#8138=ORIENTED_EDGE('',*,*,#6408,.T.);
#8139=ORIENTED_EDGE('',*,*,#6404,.F.);
#8140=ORIENTED_EDGE('',*,*,#6409,.F.);
#8141=ORIENTED_EDGE('',*,*,#6410,.T.);
#8142=ORIENTED_EDGE('',*,*,#6411,.T.);
#8143=ORIENTED_EDGE('',*,*,#6407,.F.);
#8144=ORIENTED_EDGE('',*,*,#6412,.T.);
#8145=ORIENTED_EDGE('',*,*,#6392,.T.);
#8146=ORIENTED_EDGE('',*,*,#6413,.T.);
#8147=ORIENTED_EDGE('',*,*,#6414,.F.);
#8148=ORIENTED_EDGE('',*,*,#6415,.T.);
#8149=ORIENTED_EDGE('',*,*,#6416,.T.);
#8150=ORIENTED_EDGE('',*,*,#6417,.T.);
#8151=ORIENTED_EDGE('',*,*,#6410,.F.);
#8152=ORIENTED_EDGE('',*,*,#6418,.F.);
#8153=ORIENTED_EDGE('',*,*,#6419,.T.);
#8154=ORIENTED_EDGE('',*,*,#6420,.F.);
#8155=ORIENTED_EDGE('',*,*,#6421,.F.);
#8156=ORIENTED_EDGE('',*,*,#6422,.T.);
#8157=ORIENTED_EDGE('',*,*,#6421,.T.);
#8158=ORIENTED_EDGE('',*,*,#6423,.F.);
#8159=ORIENTED_EDGE('',*,*,#6424,.F.);
#8160=ORIENTED_EDGE('',*,*,#6425,.F.);
#8161=ORIENTED_EDGE('',*,*,#6424,.T.);
#8162=ORIENTED_EDGE('',*,*,#6426,.F.);
#8163=ORIENTED_EDGE('',*,*,#6427,.F.);
#8164=ORIENTED_EDGE('',*,*,#6428,.T.);
#8165=ORIENTED_EDGE('',*,*,#6429,.F.);
#8166=ORIENTED_EDGE('',*,*,#6430,.F.);
#8167=ORIENTED_EDGE('',*,*,#6431,.F.);
#8168=ORIENTED_EDGE('',*,*,#6432,.F.);
#8169=ORIENTED_EDGE('',*,*,#6431,.T.);
#8170=ORIENTED_EDGE('',*,*,#6433,.F.);
#8171=ORIENTED_EDGE('',*,*,#6434,.F.);
#8172=ORIENTED_EDGE('',*,*,#6435,.T.);
#8173=ORIENTED_EDGE('',*,*,#6434,.T.);
#8174=ORIENTED_EDGE('',*,*,#6436,.F.);
#8175=ORIENTED_EDGE('',*,*,#6437,.F.);
#8176=ORIENTED_EDGE('',*,*,#6438,.T.);
#8177=ORIENTED_EDGE('',*,*,#6437,.T.);
#8178=ORIENTED_EDGE('',*,*,#6439,.F.);
#8179=ORIENTED_EDGE('',*,*,#6416,.F.);
#8180=ORIENTED_EDGE('',*,*,#6440,.F.);
#8181=ORIENTED_EDGE('',*,*,#6441,.F.);
#8182=ORIENTED_EDGE('',*,*,#6442,.F.);
#8183=ORIENTED_EDGE('',*,*,#6414,.T.);
#8184=ORIENTED_EDGE('',*,*,#6443,.F.);
#8185=ORIENTED_EDGE('',*,*,#6441,.T.);
#8186=ORIENTED_EDGE('',*,*,#6444,.F.);
#8187=ORIENTED_EDGE('',*,*,#6419,.F.);
#8188=ORIENTED_EDGE('',*,*,#6427,.T.);
#8189=ORIENTED_EDGE('',*,*,#6445,.F.);
#8190=ORIENTED_EDGE('',*,*,#6446,.F.);
#8191=ORIENTED_EDGE('',*,*,#6447,.T.);
#8192=ORIENTED_EDGE('',*,*,#6397,.T.);
#8193=ORIENTED_EDGE('',*,*,#6448,.T.);
#8194=ORIENTED_EDGE('',*,*,#6449,.T.);
#8195=ORIENTED_EDGE('',*,*,#6450,.F.);
#8196=ORIENTED_EDGE('',*,*,#6402,.T.);
#8197=ORIENTED_EDGE('',*,*,#6451,.F.);
#8198=ORIENTED_EDGE('',*,*,#6429,.T.);
#8199=ORIENTED_EDGE('',*,*,#6452,.T.);
#8200=ORIENTED_EDGE('',*,*,#6453,.F.);
#8201=ORIENTED_EDGE('',*,*,#6454,.T.);
#8202=ORIENTED_EDGE('',*,*,#6455,.T.);
#8203=ORIENTED_EDGE('',*,*,#6449,.F.);
#8204=ORIENTED_EDGE('',*,*,#6456,.T.);
#8205=ORIENTED_EDGE('',*,*,#6457,.T.);
#8206=ORIENTED_EDGE('',*,*,#6458,.T.);
#8207=ORIENTED_EDGE('',*,*,#6454,.F.);
#8208=ORIENTED_EDGE('',*,*,#6459,.F.);
#8209=ORIENTED_EDGE('',*,*,#6460,.T.);
#8210=ORIENTED_EDGE('',*,*,#6461,.T.);
#8211=ORIENTED_EDGE('',*,*,#6457,.F.);
#8212=ORIENTED_EDGE('',*,*,#6462,.T.);
#8213=ORIENTED_EDGE('',*,*,#6463,.T.);
#8214=ORIENTED_EDGE('',*,*,#6464,.T.);
#8215=ORIENTED_EDGE('',*,*,#6460,.F.);
#8216=ORIENTED_EDGE('',*,*,#6465,.F.);
#8217=ORIENTED_EDGE('',*,*,#6466,.T.);
#8218=ORIENTED_EDGE('',*,*,#6467,.T.);
#8219=ORIENTED_EDGE('',*,*,#6463,.F.);
#8220=ORIENTED_EDGE('',*,*,#6468,.F.);
#8221=ORIENTED_EDGE('',*,*,#6469,.T.);
#8222=ORIENTED_EDGE('',*,*,#6470,.T.);
#8223=ORIENTED_EDGE('',*,*,#6466,.F.);
#8224=ORIENTED_EDGE('',*,*,#6471,.T.);
#8225=ORIENTED_EDGE('',*,*,#6472,.T.);
#8226=ORIENTED_EDGE('',*,*,#6473,.T.);
#8227=ORIENTED_EDGE('',*,*,#6469,.F.);
#8228=ORIENTED_EDGE('',*,*,#6474,.F.);
#8229=ORIENTED_EDGE('',*,*,#6475,.T.);
#8230=ORIENTED_EDGE('',*,*,#6476,.T.);
#8231=ORIENTED_EDGE('',*,*,#6472,.F.);
#8232=ORIENTED_EDGE('',*,*,#6477,.T.);
#8233=ORIENTED_EDGE('',*,*,#6478,.T.);
#8234=ORIENTED_EDGE('',*,*,#6479,.T.);
#8235=ORIENTED_EDGE('',*,*,#6475,.F.);
#8236=ORIENTED_EDGE('',*,*,#6480,.T.);
#8237=ORIENTED_EDGE('',*,*,#6481,.T.);
#8238=ORIENTED_EDGE('',*,*,#6482,.T.);
#8239=ORIENTED_EDGE('',*,*,#6478,.F.);
#8240=ORIENTED_EDGE('',*,*,#6483,.T.);
#8241=ORIENTED_EDGE('',*,*,#6446,.T.);
#8242=ORIENTED_EDGE('',*,*,#6484,.F.);
#8243=ORIENTED_EDGE('',*,*,#6485,.F.);
#8244=ORIENTED_EDGE('',*,*,#6486,.F.);
#8245=ORIENTED_EDGE('',*,*,#6485,.T.);
#8246=ORIENTED_EDGE('',*,*,#6487,.F.);
#8247=ORIENTED_EDGE('',*,*,#6488,.F.);
#8248=ORIENTED_EDGE('',*,*,#6489,.T.);
#8249=ORIENTED_EDGE('',*,*,#6488,.T.);
#8250=ORIENTED_EDGE('',*,*,#6490,.F.);
#8251=ORIENTED_EDGE('',*,*,#6491,.F.);
#8252=ORIENTED_EDGE('',*,*,#6492,.F.);
#8253=ORIENTED_EDGE('',*,*,#6491,.T.);
#8254=ORIENTED_EDGE('',*,*,#6493,.F.);
#8255=ORIENTED_EDGE('',*,*,#6494,.F.);
#8256=ORIENTED_EDGE('',*,*,#6495,.T.);
#8257=ORIENTED_EDGE('',*,*,#6494,.T.);
#8258=ORIENTED_EDGE('',*,*,#6496,.F.);
#8259=ORIENTED_EDGE('',*,*,#6497,.F.);
#8260=ORIENTED_EDGE('',*,*,#6498,.T.);
#8261=ORIENTED_EDGE('',*,*,#6497,.T.);
#8262=ORIENTED_EDGE('',*,*,#6499,.F.);
#8263=ORIENTED_EDGE('',*,*,#6500,.F.);
#8264=ORIENTED_EDGE('',*,*,#6501,.F.);
#8265=ORIENTED_EDGE('',*,*,#6500,.T.);
#8266=ORIENTED_EDGE('',*,*,#6502,.F.);
#8267=ORIENTED_EDGE('',*,*,#6503,.F.);
#8268=ORIENTED_EDGE('',*,*,#6504,.T.);
#8269=ORIENTED_EDGE('',*,*,#6503,.T.);
#8270=ORIENTED_EDGE('',*,*,#6505,.F.);
#8271=ORIENTED_EDGE('',*,*,#6506,.F.);
#8272=ORIENTED_EDGE('',*,*,#6507,.F.);
#8273=ORIENTED_EDGE('',*,*,#6506,.T.);
#8274=ORIENTED_EDGE('',*,*,#6508,.F.);
#8275=ORIENTED_EDGE('',*,*,#6481,.F.);
#8276=ORIENTED_EDGE('',*,*,#6396,.F.);
#8277=ORIENTED_EDGE('',*,*,#6393,.T.);
#8278=ORIENTED_EDGE('',*,*,#6389,.F.);
#8279=ORIENTED_EDGE('',*,*,#6412,.F.);
#8280=ORIENTED_EDGE('',*,*,#6442,.T.);
#8281=ORIENTED_EDGE('',*,*,#6443,.T.);
#8282=ORIENTED_EDGE('',*,*,#6418,.T.);
#8283=ORIENTED_EDGE('',*,*,#6422,.F.);
#8284=ORIENTED_EDGE('',*,*,#6425,.T.);
#8285=ORIENTED_EDGE('',*,*,#6447,.F.);
#8286=ORIENTED_EDGE('',*,*,#6483,.F.);
#8287=ORIENTED_EDGE('',*,*,#6486,.T.);
#8288=ORIENTED_EDGE('',*,*,#6489,.F.);
#8289=ORIENTED_EDGE('',*,*,#6492,.T.);
#8290=ORIENTED_EDGE('',*,*,#6495,.F.);
#8291=ORIENTED_EDGE('',*,*,#6498,.F.);
#8292=ORIENTED_EDGE('',*,*,#6501,.T.);
#8293=ORIENTED_EDGE('',*,*,#6504,.F.);
#8294=ORIENTED_EDGE('',*,*,#6507,.T.);
#8295=ORIENTED_EDGE('',*,*,#6480,.F.);
#8296=ORIENTED_EDGE('',*,*,#6477,.F.);
#8297=ORIENTED_EDGE('',*,*,#6474,.T.);
#8298=ORIENTED_EDGE('',*,*,#6471,.F.);
#8299=ORIENTED_EDGE('',*,*,#6468,.T.);
#8300=ORIENTED_EDGE('',*,*,#6465,.T.);
#8301=ORIENTED_EDGE('',*,*,#6462,.F.);
#8302=ORIENTED_EDGE('',*,*,#6459,.T.);
#8303=ORIENTED_EDGE('',*,*,#6456,.F.);
#8304=ORIENTED_EDGE('',*,*,#6453,.T.);
#8305=ORIENTED_EDGE('',*,*,#6448,.F.);
#8306=ORIENTED_EDGE('',*,*,#6452,.F.);
#8307=ORIENTED_EDGE('',*,*,#6428,.F.);
#8308=ORIENTED_EDGE('',*,*,#6432,.T.);
#8309=ORIENTED_EDGE('',*,*,#6435,.F.);
#8310=ORIENTED_EDGE('',*,*,#6438,.F.);
#8311=ORIENTED_EDGE('',*,*,#6415,.F.);
#8312=ORIENTED_EDGE('',*,*,#6409,.T.);
#8313=ORIENTED_EDGE('',*,*,#6406,.T.);
#8314=ORIENTED_EDGE('',*,*,#6403,.F.);
#8315=ORIENTED_EDGE('',*,*,#6399,.T.);
#8316=ORIENTED_EDGE('',*,*,#6450,.T.);
#8317=ORIENTED_EDGE('',*,*,#6455,.F.);
#8318=ORIENTED_EDGE('',*,*,#6458,.F.);
#8319=ORIENTED_EDGE('',*,*,#6461,.F.);
#8320=ORIENTED_EDGE('',*,*,#6464,.F.);
#8321=ORIENTED_EDGE('',*,*,#6467,.F.);
#8322=ORIENTED_EDGE('',*,*,#6470,.F.);
#8323=ORIENTED_EDGE('',*,*,#6473,.F.);
#8324=ORIENTED_EDGE('',*,*,#6476,.F.);
#8325=ORIENTED_EDGE('',*,*,#6479,.F.);
#8326=ORIENTED_EDGE('',*,*,#6482,.F.);
#8327=ORIENTED_EDGE('',*,*,#6508,.T.);
#8328=ORIENTED_EDGE('',*,*,#6505,.T.);
#8329=ORIENTED_EDGE('',*,*,#6502,.T.);
#8330=ORIENTED_EDGE('',*,*,#6499,.T.);
#8331=ORIENTED_EDGE('',*,*,#6496,.T.);
#8332=ORIENTED_EDGE('',*,*,#6493,.T.);
#8333=ORIENTED_EDGE('',*,*,#6490,.T.);
#8334=ORIENTED_EDGE('',*,*,#6487,.T.);
#8335=ORIENTED_EDGE('',*,*,#6484,.T.);
#8336=ORIENTED_EDGE('',*,*,#6445,.T.);
#8337=ORIENTED_EDGE('',*,*,#6426,.T.);
#8338=ORIENTED_EDGE('',*,*,#6423,.T.);
#8339=ORIENTED_EDGE('',*,*,#6420,.T.);
#8340=ORIENTED_EDGE('',*,*,#6444,.T.);
#8341=ORIENTED_EDGE('',*,*,#6440,.T.);
#8342=ORIENTED_EDGE('',*,*,#6413,.F.);
#8343=ORIENTED_EDGE('',*,*,#6391,.F.);
#8344=ORIENTED_EDGE('',*,*,#6395,.F.);
#8345=ORIENTED_EDGE('',*,*,#6398,.F.);
#8346=ORIENTED_EDGE('',*,*,#6401,.F.);
#8347=ORIENTED_EDGE('',*,*,#6405,.F.);
#8348=ORIENTED_EDGE('',*,*,#6408,.F.);
#8349=ORIENTED_EDGE('',*,*,#6411,.F.);
#8350=ORIENTED_EDGE('',*,*,#6417,.F.);
#8351=ORIENTED_EDGE('',*,*,#6439,.T.);
#8352=ORIENTED_EDGE('',*,*,#6436,.T.);
#8353=ORIENTED_EDGE('',*,*,#6433,.T.);
#8354=ORIENTED_EDGE('',*,*,#6430,.T.);
#8355=ORIENTED_EDGE('',*,*,#6451,.T.);
#8356=ORIENTED_EDGE('',*,*,#6509,.F.);
#8357=ORIENTED_EDGE('',*,*,#6510,.T.);
#8358=ORIENTED_EDGE('',*,*,#6511,.F.);
#8359=ORIENTED_EDGE('',*,*,#6510,.F.);
#8360=ORIENTED_EDGE('',*,*,#6512,.F.);
#8361=ORIENTED_EDGE('',*,*,#6513,.T.);
#8362=ORIENTED_EDGE('',*,*,#6514,.F.);
#8363=ORIENTED_EDGE('',*,*,#6513,.F.);
#8364=ORIENTED_EDGE('',*,*,#6515,.F.);
#8365=ORIENTED_EDGE('',*,*,#6516,.T.);
#8366=ORIENTED_EDGE('',*,*,#6517,.F.);
#8367=ORIENTED_EDGE('',*,*,#6516,.F.);
#8368=ORIENTED_EDGE('',*,*,#6518,.F.);
#8369=ORIENTED_EDGE('',*,*,#6519,.T.);
#8370=ORIENTED_EDGE('',*,*,#6520,.F.);
#8371=ORIENTED_EDGE('',*,*,#6519,.F.);
#8372=ORIENTED_EDGE('',*,*,#6521,.F.);
#8373=ORIENTED_EDGE('',*,*,#6522,.T.);
#8374=ORIENTED_EDGE('',*,*,#6523,.F.);
#8375=ORIENTED_EDGE('',*,*,#6522,.F.);
#8376=ORIENTED_EDGE('',*,*,#6524,.F.);
#8377=ORIENTED_EDGE('',*,*,#6525,.F.);
#8378=ORIENTED_EDGE('',*,*,#6526,.F.);
#8379=ORIENTED_EDGE('',*,*,#6527,.T.);
#8380=ORIENTED_EDGE('',*,*,#6528,.F.);
#8381=ORIENTED_EDGE('',*,*,#6527,.F.);
#8382=ORIENTED_EDGE('',*,*,#6529,.F.);
#8383=ORIENTED_EDGE('',*,*,#6530,.T.);
#8384=ORIENTED_EDGE('',*,*,#6531,.F.);
#8385=ORIENTED_EDGE('',*,*,#6530,.F.);
#8386=ORIENTED_EDGE('',*,*,#6532,.F.);
#8387=ORIENTED_EDGE('',*,*,#6533,.T.);
#8388=ORIENTED_EDGE('',*,*,#6534,.F.);
#8389=ORIENTED_EDGE('',*,*,#6533,.F.);
#8390=ORIENTED_EDGE('',*,*,#6535,.F.);
#8391=ORIENTED_EDGE('',*,*,#6525,.T.);
#8392=ORIENTED_EDGE('',*,*,#6536,.F.);
#8393=ORIENTED_EDGE('',*,*,#6537,.F.);
#8394=ORIENTED_EDGE('',*,*,#6538,.F.);
#8395=ORIENTED_EDGE('',*,*,#6539,.T.);
#8396=ORIENTED_EDGE('',*,*,#6540,.F.);
#8397=ORIENTED_EDGE('',*,*,#6539,.F.);
#8398=ORIENTED_EDGE('',*,*,#6541,.F.);
#8399=ORIENTED_EDGE('',*,*,#6542,.T.);
#8400=ORIENTED_EDGE('',*,*,#6543,.F.);
#8401=ORIENTED_EDGE('',*,*,#6542,.F.);
#8402=ORIENTED_EDGE('',*,*,#6544,.F.);
#8403=ORIENTED_EDGE('',*,*,#6545,.T.);
#8404=ORIENTED_EDGE('',*,*,#6546,.F.);
#8405=ORIENTED_EDGE('',*,*,#6545,.F.);
#8406=ORIENTED_EDGE('',*,*,#6547,.F.);
#8407=ORIENTED_EDGE('',*,*,#6537,.T.);
#8408=ORIENTED_EDGE('',*,*,#6548,.F.);
#8409=ORIENTED_EDGE('',*,*,#6549,.T.);
#8410=ORIENTED_EDGE('',*,*,#6550,.F.);
#8411=ORIENTED_EDGE('',*,*,#6549,.F.);
#8412=ORIENTED_EDGE('',*,*,#6551,.F.);
#8413=ORIENTED_EDGE('',*,*,#6552,.T.);
#8414=ORIENTED_EDGE('',*,*,#6553,.F.);
#8415=ORIENTED_EDGE('',*,*,#6552,.F.);
#8416=ORIENTED_EDGE('',*,*,#6554,.F.);
#8417=ORIENTED_EDGE('',*,*,#6555,.T.);
#8418=ORIENTED_EDGE('',*,*,#6556,.F.);
#8419=ORIENTED_EDGE('',*,*,#6555,.F.);
#8420=ORIENTED_EDGE('',*,*,#6557,.F.);
#8421=ORIENTED_EDGE('',*,*,#6558,.T.);
#8422=ORIENTED_EDGE('',*,*,#6559,.F.);
#8423=ORIENTED_EDGE('',*,*,#6558,.F.);
#8424=ORIENTED_EDGE('',*,*,#6560,.F.);
#8425=ORIENTED_EDGE('',*,*,#6561,.T.);
#8426=ORIENTED_EDGE('',*,*,#6562,.F.);
#8427=ORIENTED_EDGE('',*,*,#6561,.F.);
#8428=ORIENTED_EDGE('',*,*,#6563,.F.);
#8429=ORIENTED_EDGE('',*,*,#6564,.F.);
#8430=ORIENTED_EDGE('',*,*,#6565,.F.);
#8431=ORIENTED_EDGE('',*,*,#6566,.T.);
#8432=ORIENTED_EDGE('',*,*,#6567,.F.);
#8433=ORIENTED_EDGE('',*,*,#6566,.F.);
#8434=ORIENTED_EDGE('',*,*,#6568,.F.);
#8435=ORIENTED_EDGE('',*,*,#6569,.T.);
#8436=ORIENTED_EDGE('',*,*,#6570,.F.);
#8437=ORIENTED_EDGE('',*,*,#6569,.F.);
#8438=ORIENTED_EDGE('',*,*,#6571,.F.);
#8439=ORIENTED_EDGE('',*,*,#6572,.T.);
#8440=ORIENTED_EDGE('',*,*,#6573,.F.);
#8441=ORIENTED_EDGE('',*,*,#6572,.F.);
#8442=ORIENTED_EDGE('',*,*,#6574,.F.);
#8443=ORIENTED_EDGE('',*,*,#6564,.T.);
#8444=ORIENTED_EDGE('',*,*,#6575,.F.);
#8445=ORIENTED_EDGE('',*,*,#6576,.F.);
#8446=ORIENTED_EDGE('',*,*,#6577,.F.);
#8447=ORIENTED_EDGE('',*,*,#6578,.T.);
#8448=ORIENTED_EDGE('',*,*,#6579,.F.);
#8449=ORIENTED_EDGE('',*,*,#6578,.F.);
#8450=ORIENTED_EDGE('',*,*,#6580,.F.);
#8451=ORIENTED_EDGE('',*,*,#6581,.T.);
#8452=ORIENTED_EDGE('',*,*,#6582,.F.);
#8453=ORIENTED_EDGE('',*,*,#6581,.F.);
#8454=ORIENTED_EDGE('',*,*,#6583,.F.);
#8455=ORIENTED_EDGE('',*,*,#6584,.T.);
#8456=ORIENTED_EDGE('',*,*,#6585,.F.);
#8457=ORIENTED_EDGE('',*,*,#6584,.F.);
#8458=ORIENTED_EDGE('',*,*,#6586,.F.);
#8459=ORIENTED_EDGE('',*,*,#6576,.T.);
#8460=ORIENTED_EDGE('',*,*,#6587,.F.);
#8461=ORIENTED_EDGE('',*,*,#6588,.T.);
#8462=ORIENTED_EDGE('',*,*,#6589,.F.);
#8463=ORIENTED_EDGE('',*,*,#6588,.F.);
#8464=ORIENTED_EDGE('',*,*,#6590,.F.);
#8465=ORIENTED_EDGE('',*,*,#6591,.T.);
#8466=ORIENTED_EDGE('',*,*,#6592,.F.);
#8467=ORIENTED_EDGE('',*,*,#6591,.F.);
#8468=ORIENTED_EDGE('',*,*,#6593,.F.);
#8469=ORIENTED_EDGE('',*,*,#6594,.T.);
#8470=ORIENTED_EDGE('',*,*,#6595,.F.);
#8471=ORIENTED_EDGE('',*,*,#6594,.F.);
#8472=ORIENTED_EDGE('',*,*,#6596,.F.);
#8473=ORIENTED_EDGE('',*,*,#6597,.T.);
#8474=ORIENTED_EDGE('',*,*,#6598,.F.);
#8475=ORIENTED_EDGE('',*,*,#6597,.F.);
#8476=ORIENTED_EDGE('',*,*,#6599,.F.);
#8477=ORIENTED_EDGE('',*,*,#6600,.T.);
#8478=ORIENTED_EDGE('',*,*,#6601,.F.);
#8479=ORIENTED_EDGE('',*,*,#6600,.F.);
#8480=ORIENTED_EDGE('',*,*,#6602,.F.);
#8481=ORIENTED_EDGE('',*,*,#6603,.F.);
#8482=ORIENTED_EDGE('',*,*,#6604,.F.);
#8483=ORIENTED_EDGE('',*,*,#6605,.T.);
#8484=ORIENTED_EDGE('',*,*,#6606,.F.);
#8485=ORIENTED_EDGE('',*,*,#6605,.F.);
#8486=ORIENTED_EDGE('',*,*,#6607,.F.);
#8487=ORIENTED_EDGE('',*,*,#6608,.T.);
#8488=ORIENTED_EDGE('',*,*,#6609,.F.);
#8489=ORIENTED_EDGE('',*,*,#6608,.F.);
#8490=ORIENTED_EDGE('',*,*,#6610,.F.);
#8491=ORIENTED_EDGE('',*,*,#6611,.T.);
#8492=ORIENTED_EDGE('',*,*,#6612,.F.);
#8493=ORIENTED_EDGE('',*,*,#6611,.F.);
#8494=ORIENTED_EDGE('',*,*,#6613,.F.);
#8495=ORIENTED_EDGE('',*,*,#6603,.T.);
#8496=ORIENTED_EDGE('',*,*,#6614,.F.);
#8497=ORIENTED_EDGE('',*,*,#6615,.F.);
#8498=ORIENTED_EDGE('',*,*,#6616,.F.);
#8499=ORIENTED_EDGE('',*,*,#6617,.T.);
#8500=ORIENTED_EDGE('',*,*,#6618,.F.);
#8501=ORIENTED_EDGE('',*,*,#6617,.F.);
#8502=ORIENTED_EDGE('',*,*,#6619,.F.);
#8503=ORIENTED_EDGE('',*,*,#6620,.T.);
#8504=ORIENTED_EDGE('',*,*,#6621,.F.);
#8505=ORIENTED_EDGE('',*,*,#6620,.F.);
#8506=ORIENTED_EDGE('',*,*,#6622,.F.);
#8507=ORIENTED_EDGE('',*,*,#6623,.T.);
#8508=ORIENTED_EDGE('',*,*,#6624,.F.);
#8509=ORIENTED_EDGE('',*,*,#6623,.F.);
#8510=ORIENTED_EDGE('',*,*,#6625,.F.);
#8511=ORIENTED_EDGE('',*,*,#6615,.T.);
#8512=ORIENTED_EDGE('',*,*,#6626,.F.);
#8513=ORIENTED_EDGE('',*,*,#6627,.T.);
#8514=ORIENTED_EDGE('',*,*,#6628,.F.);
#8515=ORIENTED_EDGE('',*,*,#6627,.F.);
#8516=ORIENTED_EDGE('',*,*,#6629,.F.);
#8517=ORIENTED_EDGE('',*,*,#6630,.T.);
#8518=ORIENTED_EDGE('',*,*,#6631,.F.);
#8519=ORIENTED_EDGE('',*,*,#6630,.F.);
#8520=ORIENTED_EDGE('',*,*,#6632,.F.);
#8521=ORIENTED_EDGE('',*,*,#6633,.T.);
#8522=ORIENTED_EDGE('',*,*,#6634,.F.);
#8523=ORIENTED_EDGE('',*,*,#6633,.F.);
#8524=ORIENTED_EDGE('',*,*,#6635,.F.);
#8525=ORIENTED_EDGE('',*,*,#6636,.T.);
#8526=ORIENTED_EDGE('',*,*,#6637,.F.);
#8527=ORIENTED_EDGE('',*,*,#6636,.F.);
#8528=ORIENTED_EDGE('',*,*,#6638,.F.);
#8529=ORIENTED_EDGE('',*,*,#6639,.T.);
#8530=ORIENTED_EDGE('',*,*,#6640,.F.);
#8531=ORIENTED_EDGE('',*,*,#6639,.F.);
#8532=ORIENTED_EDGE('',*,*,#6641,.F.);
#8533=ORIENTED_EDGE('',*,*,#6642,.F.);
#8534=ORIENTED_EDGE('',*,*,#6643,.F.);
#8535=ORIENTED_EDGE('',*,*,#6644,.T.);
#8536=ORIENTED_EDGE('',*,*,#6645,.F.);
#8537=ORIENTED_EDGE('',*,*,#6644,.F.);
#8538=ORIENTED_EDGE('',*,*,#6646,.F.);
#8539=ORIENTED_EDGE('',*,*,#6647,.T.);
#8540=ORIENTED_EDGE('',*,*,#6648,.F.);
#8541=ORIENTED_EDGE('',*,*,#6647,.F.);
#8542=ORIENTED_EDGE('',*,*,#6649,.F.);
#8543=ORIENTED_EDGE('',*,*,#6650,.T.);
#8544=ORIENTED_EDGE('',*,*,#6651,.F.);
#8545=ORIENTED_EDGE('',*,*,#6650,.F.);
#8546=ORIENTED_EDGE('',*,*,#6652,.F.);
#8547=ORIENTED_EDGE('',*,*,#6642,.T.);
#8548=ORIENTED_EDGE('',*,*,#6653,.F.);
#8549=ORIENTED_EDGE('',*,*,#6654,.F.);
#8550=ORIENTED_EDGE('',*,*,#6655,.F.);
#8551=ORIENTED_EDGE('',*,*,#6656,.T.);
#8552=ORIENTED_EDGE('',*,*,#6657,.F.);
#8553=ORIENTED_EDGE('',*,*,#6656,.F.);
#8554=ORIENTED_EDGE('',*,*,#6658,.F.);
#8555=ORIENTED_EDGE('',*,*,#6659,.T.);
#8556=ORIENTED_EDGE('',*,*,#6660,.F.);
#8557=ORIENTED_EDGE('',*,*,#6659,.F.);
#8558=ORIENTED_EDGE('',*,*,#6661,.F.);
#8559=ORIENTED_EDGE('',*,*,#6662,.T.);
#8560=ORIENTED_EDGE('',*,*,#6663,.F.);
#8561=ORIENTED_EDGE('',*,*,#6662,.F.);
#8562=ORIENTED_EDGE('',*,*,#6664,.F.);
#8563=ORIENTED_EDGE('',*,*,#6654,.T.);
#8564=ORIENTED_EDGE('',*,*,#6665,.F.);
#8565=ORIENTED_EDGE('',*,*,#6666,.T.);
#8566=ORIENTED_EDGE('',*,*,#6667,.F.);
#8567=ORIENTED_EDGE('',*,*,#6666,.F.);
#8568=ORIENTED_EDGE('',*,*,#6668,.F.);
#8569=ORIENTED_EDGE('',*,*,#6669,.T.);
#8570=ORIENTED_EDGE('',*,*,#6670,.F.);
#8571=ORIENTED_EDGE('',*,*,#6669,.F.);
#8572=ORIENTED_EDGE('',*,*,#6671,.F.);
#8573=ORIENTED_EDGE('',*,*,#6672,.T.);
#8574=ORIENTED_EDGE('',*,*,#6673,.F.);
#8575=ORIENTED_EDGE('',*,*,#6672,.F.);
#8576=ORIENTED_EDGE('',*,*,#6674,.F.);
#8577=ORIENTED_EDGE('',*,*,#6675,.T.);
#8578=ORIENTED_EDGE('',*,*,#6676,.F.);
#8579=ORIENTED_EDGE('',*,*,#6675,.F.);
#8580=ORIENTED_EDGE('',*,*,#6677,.F.);
#8581=ORIENTED_EDGE('',*,*,#6678,.T.);
#8582=ORIENTED_EDGE('',*,*,#6679,.F.);
#8583=ORIENTED_EDGE('',*,*,#6678,.F.);
#8584=ORIENTED_EDGE('',*,*,#6680,.F.);
#8585=ORIENTED_EDGE('',*,*,#6681,.F.);
#8586=ORIENTED_EDGE('',*,*,#6682,.F.);
#8587=ORIENTED_EDGE('',*,*,#6683,.T.);
#8588=ORIENTED_EDGE('',*,*,#6684,.F.);
#8589=ORIENTED_EDGE('',*,*,#6683,.F.);
#8590=ORIENTED_EDGE('',*,*,#6685,.F.);
#8591=ORIENTED_EDGE('',*,*,#6686,.T.);
#8592=ORIENTED_EDGE('',*,*,#6687,.F.);
#8593=ORIENTED_EDGE('',*,*,#6686,.F.);
#8594=ORIENTED_EDGE('',*,*,#6688,.F.);
#8595=ORIENTED_EDGE('',*,*,#6689,.T.);
#8596=ORIENTED_EDGE('',*,*,#6690,.F.);
#8597=ORIENTED_EDGE('',*,*,#6689,.F.);
#8598=ORIENTED_EDGE('',*,*,#6691,.F.);
#8599=ORIENTED_EDGE('',*,*,#6681,.T.);
#8600=ORIENTED_EDGE('',*,*,#6692,.F.);
#8601=ORIENTED_EDGE('',*,*,#6693,.F.);
#8602=ORIENTED_EDGE('',*,*,#6694,.F.);
#8603=ORIENTED_EDGE('',*,*,#6695,.T.);
#8604=ORIENTED_EDGE('',*,*,#6696,.F.);
#8605=ORIENTED_EDGE('',*,*,#6695,.F.);
#8606=ORIENTED_EDGE('',*,*,#6697,.F.);
#8607=ORIENTED_EDGE('',*,*,#6698,.T.);
#8608=ORIENTED_EDGE('',*,*,#6699,.F.);
#8609=ORIENTED_EDGE('',*,*,#6698,.F.);
#8610=ORIENTED_EDGE('',*,*,#6700,.F.);
#8611=ORIENTED_EDGE('',*,*,#6701,.T.);
#8612=ORIENTED_EDGE('',*,*,#6702,.F.);
#8613=ORIENTED_EDGE('',*,*,#6701,.F.);
#8614=ORIENTED_EDGE('',*,*,#6703,.F.);
#8615=ORIENTED_EDGE('',*,*,#6693,.T.);
#8616=ORIENTED_EDGE('',*,*,#6704,.F.);
#8617=ORIENTED_EDGE('',*,*,#6705,.T.);
#8618=ORIENTED_EDGE('',*,*,#6706,.F.);
#8619=ORIENTED_EDGE('',*,*,#6705,.F.);
#8620=ORIENTED_EDGE('',*,*,#6707,.F.);
#8621=ORIENTED_EDGE('',*,*,#6708,.T.);
#8622=ORIENTED_EDGE('',*,*,#6709,.F.);
#8623=ORIENTED_EDGE('',*,*,#6708,.F.);
#8624=ORIENTED_EDGE('',*,*,#6710,.F.);
#8625=ORIENTED_EDGE('',*,*,#6711,.T.);
#8626=ORIENTED_EDGE('',*,*,#6712,.F.);
#8627=ORIENTED_EDGE('',*,*,#6711,.F.);
#8628=ORIENTED_EDGE('',*,*,#6713,.F.);
#8629=ORIENTED_EDGE('',*,*,#6714,.T.);
#8630=ORIENTED_EDGE('',*,*,#6715,.F.);
#8631=ORIENTED_EDGE('',*,*,#6714,.F.);
#8632=ORIENTED_EDGE('',*,*,#6716,.F.);
#8633=ORIENTED_EDGE('',*,*,#6717,.T.);
#8634=ORIENTED_EDGE('',*,*,#6718,.F.);
#8635=ORIENTED_EDGE('',*,*,#6717,.F.);
#8636=ORIENTED_EDGE('',*,*,#6719,.F.);
#8637=ORIENTED_EDGE('',*,*,#6720,.F.);
#8638=ORIENTED_EDGE('',*,*,#6721,.F.);
#8639=ORIENTED_EDGE('',*,*,#6722,.T.);
#8640=ORIENTED_EDGE('',*,*,#6723,.F.);
#8641=ORIENTED_EDGE('',*,*,#6722,.F.);
#8642=ORIENTED_EDGE('',*,*,#6724,.F.);
#8643=ORIENTED_EDGE('',*,*,#6725,.T.);
#8644=ORIENTED_EDGE('',*,*,#6726,.F.);
#8645=ORIENTED_EDGE('',*,*,#6725,.F.);
#8646=ORIENTED_EDGE('',*,*,#6727,.F.);
#8647=ORIENTED_EDGE('',*,*,#6728,.T.);
#8648=ORIENTED_EDGE('',*,*,#6729,.F.);
#8649=ORIENTED_EDGE('',*,*,#6728,.F.);
#8650=ORIENTED_EDGE('',*,*,#6730,.F.);
#8651=ORIENTED_EDGE('',*,*,#6720,.T.);
#8652=ORIENTED_EDGE('',*,*,#6731,.F.);
#8653=ORIENTED_EDGE('',*,*,#6732,.F.);
#8654=ORIENTED_EDGE('',*,*,#6733,.F.);
#8655=ORIENTED_EDGE('',*,*,#6734,.T.);
#8656=ORIENTED_EDGE('',*,*,#6735,.F.);
#8657=ORIENTED_EDGE('',*,*,#6734,.F.);
#8658=ORIENTED_EDGE('',*,*,#6736,.F.);
#8659=ORIENTED_EDGE('',*,*,#6737,.T.);
#8660=ORIENTED_EDGE('',*,*,#6738,.F.);
#8661=ORIENTED_EDGE('',*,*,#6737,.F.);
#8662=ORIENTED_EDGE('',*,*,#6739,.F.);
#8663=ORIENTED_EDGE('',*,*,#6740,.T.);
#8664=ORIENTED_EDGE('',*,*,#6741,.F.);
#8665=ORIENTED_EDGE('',*,*,#6740,.F.);
#8666=ORIENTED_EDGE('',*,*,#6742,.F.);
#8667=ORIENTED_EDGE('',*,*,#6732,.T.);
#8668=ORIENTED_EDGE('',*,*,#6743,.F.);
#8669=ORIENTED_EDGE('',*,*,#6744,.T.);
#8670=ORIENTED_EDGE('',*,*,#6745,.F.);
#8671=ORIENTED_EDGE('',*,*,#6744,.F.);
#8672=ORIENTED_EDGE('',*,*,#6746,.F.);
#8673=ORIENTED_EDGE('',*,*,#6747,.T.);
#8674=ORIENTED_EDGE('',*,*,#6748,.F.);
#8675=ORIENTED_EDGE('',*,*,#6747,.F.);
#8676=ORIENTED_EDGE('',*,*,#6749,.F.);
#8677=ORIENTED_EDGE('',*,*,#6750,.T.);
#8678=ORIENTED_EDGE('',*,*,#6751,.F.);
#8679=ORIENTED_EDGE('',*,*,#6750,.F.);
#8680=ORIENTED_EDGE('',*,*,#6752,.F.);
#8681=ORIENTED_EDGE('',*,*,#6753,.T.);
#8682=ORIENTED_EDGE('',*,*,#6754,.F.);
#8683=ORIENTED_EDGE('',*,*,#6753,.F.);
#8684=ORIENTED_EDGE('',*,*,#6755,.F.);
#8685=ORIENTED_EDGE('',*,*,#6756,.T.);
#8686=ORIENTED_EDGE('',*,*,#6757,.F.);
#8687=ORIENTED_EDGE('',*,*,#6756,.F.);
#8688=ORIENTED_EDGE('',*,*,#6758,.F.);
#8689=ORIENTED_EDGE('',*,*,#6759,.F.);
#8690=ORIENTED_EDGE('',*,*,#6760,.F.);
#8691=ORIENTED_EDGE('',*,*,#6761,.T.);
#8692=ORIENTED_EDGE('',*,*,#6762,.F.);
#8693=ORIENTED_EDGE('',*,*,#6761,.F.);
#8694=ORIENTED_EDGE('',*,*,#6763,.F.);
#8695=ORIENTED_EDGE('',*,*,#6764,.T.);
#8696=ORIENTED_EDGE('',*,*,#6765,.F.);
#8697=ORIENTED_EDGE('',*,*,#6764,.F.);
#8698=ORIENTED_EDGE('',*,*,#6766,.F.);
#8699=ORIENTED_EDGE('',*,*,#6767,.T.);
#8700=ORIENTED_EDGE('',*,*,#6768,.F.);
#8701=ORIENTED_EDGE('',*,*,#6767,.F.);
#8702=ORIENTED_EDGE('',*,*,#6769,.F.);
#8703=ORIENTED_EDGE('',*,*,#6759,.T.);
#8704=ORIENTED_EDGE('',*,*,#6770,.F.);
#8705=ORIENTED_EDGE('',*,*,#6771,.F.);
#8706=ORIENTED_EDGE('',*,*,#6772,.F.);
#8707=ORIENTED_EDGE('',*,*,#6773,.T.);
#8708=ORIENTED_EDGE('',*,*,#6774,.F.);
#8709=ORIENTED_EDGE('',*,*,#6773,.F.);
#8710=ORIENTED_EDGE('',*,*,#6775,.F.);
#8711=ORIENTED_EDGE('',*,*,#6776,.T.);
#8712=ORIENTED_EDGE('',*,*,#6777,.F.);
#8713=ORIENTED_EDGE('',*,*,#6776,.F.);
#8714=ORIENTED_EDGE('',*,*,#6778,.F.);
#8715=ORIENTED_EDGE('',*,*,#6779,.T.);
#8716=ORIENTED_EDGE('',*,*,#6780,.F.);
#8717=ORIENTED_EDGE('',*,*,#6779,.F.);
#8718=ORIENTED_EDGE('',*,*,#6781,.F.);
#8719=ORIENTED_EDGE('',*,*,#6771,.T.);
#8720=ORIENTED_EDGE('',*,*,#6782,.F.);
#8721=ORIENTED_EDGE('',*,*,#6783,.T.);
#8722=ORIENTED_EDGE('',*,*,#6784,.F.);
#8723=ORIENTED_EDGE('',*,*,#6783,.F.);
#8724=ORIENTED_EDGE('',*,*,#6785,.F.);
#8725=ORIENTED_EDGE('',*,*,#6786,.T.);
#8726=ORIENTED_EDGE('',*,*,#6787,.F.);
#8727=ORIENTED_EDGE('',*,*,#6786,.F.);
#8728=ORIENTED_EDGE('',*,*,#6788,.F.);
#8729=ORIENTED_EDGE('',*,*,#6789,.T.);
#8730=ORIENTED_EDGE('',*,*,#6790,.F.);
#8731=ORIENTED_EDGE('',*,*,#6789,.F.);
#8732=ORIENTED_EDGE('',*,*,#6791,.F.);
#8733=ORIENTED_EDGE('',*,*,#6792,.T.);
#8734=ORIENTED_EDGE('',*,*,#6793,.F.);
#8735=ORIENTED_EDGE('',*,*,#6792,.F.);
#8736=ORIENTED_EDGE('',*,*,#6794,.F.);
#8737=ORIENTED_EDGE('',*,*,#6795,.T.);
#8738=ORIENTED_EDGE('',*,*,#6796,.F.);
#8739=ORIENTED_EDGE('',*,*,#6795,.F.);
#8740=ORIENTED_EDGE('',*,*,#6797,.F.);
#8741=ORIENTED_EDGE('',*,*,#6798,.F.);
#8742=ORIENTED_EDGE('',*,*,#6799,.F.);
#8743=ORIENTED_EDGE('',*,*,#6800,.T.);
#8744=ORIENTED_EDGE('',*,*,#6801,.F.);
#8745=ORIENTED_EDGE('',*,*,#6800,.F.);
#8746=ORIENTED_EDGE('',*,*,#6802,.F.);
#8747=ORIENTED_EDGE('',*,*,#6803,.T.);
#8748=ORIENTED_EDGE('',*,*,#6804,.F.);
#8749=ORIENTED_EDGE('',*,*,#6803,.F.);
#8750=ORIENTED_EDGE('',*,*,#6805,.F.);
#8751=ORIENTED_EDGE('',*,*,#6806,.T.);
#8752=ORIENTED_EDGE('',*,*,#6807,.F.);
#8753=ORIENTED_EDGE('',*,*,#6806,.F.);
#8754=ORIENTED_EDGE('',*,*,#6808,.F.);
#8755=ORIENTED_EDGE('',*,*,#6798,.T.);
#8756=ORIENTED_EDGE('',*,*,#6809,.F.);
#8757=ORIENTED_EDGE('',*,*,#6810,.F.);
#8758=ORIENTED_EDGE('',*,*,#6811,.F.);
#8759=ORIENTED_EDGE('',*,*,#6812,.T.);
#8760=ORIENTED_EDGE('',*,*,#6813,.F.);
#8761=ORIENTED_EDGE('',*,*,#6812,.F.);
#8762=ORIENTED_EDGE('',*,*,#6814,.F.);
#8763=ORIENTED_EDGE('',*,*,#6815,.T.);
#8764=ORIENTED_EDGE('',*,*,#6816,.F.);
#8765=ORIENTED_EDGE('',*,*,#6815,.F.);
#8766=ORIENTED_EDGE('',*,*,#6817,.F.);
#8767=ORIENTED_EDGE('',*,*,#6818,.T.);
#8768=ORIENTED_EDGE('',*,*,#6819,.F.);
#8769=ORIENTED_EDGE('',*,*,#6818,.F.);
#8770=ORIENTED_EDGE('',*,*,#6820,.F.);
#8771=ORIENTED_EDGE('',*,*,#6810,.T.);
#8772=ORIENTED_EDGE('',*,*,#6821,.F.);
#8773=ORIENTED_EDGE('',*,*,#6822,.T.);
#8774=ORIENTED_EDGE('',*,*,#6823,.F.);
#8775=ORIENTED_EDGE('',*,*,#6822,.F.);
#8776=ORIENTED_EDGE('',*,*,#6824,.F.);
#8777=ORIENTED_EDGE('',*,*,#6825,.T.);
#8778=ORIENTED_EDGE('',*,*,#6826,.F.);
#8779=ORIENTED_EDGE('',*,*,#6825,.F.);
#8780=ORIENTED_EDGE('',*,*,#6827,.F.);
#8781=ORIENTED_EDGE('',*,*,#6828,.T.);
#8782=ORIENTED_EDGE('',*,*,#6829,.F.);
#8783=ORIENTED_EDGE('',*,*,#6828,.F.);
#8784=ORIENTED_EDGE('',*,*,#6830,.F.);
#8785=ORIENTED_EDGE('',*,*,#6831,.T.);
#8786=ORIENTED_EDGE('',*,*,#6832,.F.);
#8787=ORIENTED_EDGE('',*,*,#6831,.F.);
#8788=ORIENTED_EDGE('',*,*,#6833,.F.);
#8789=ORIENTED_EDGE('',*,*,#6834,.T.);
#8790=ORIENTED_EDGE('',*,*,#6835,.F.);
#8791=ORIENTED_EDGE('',*,*,#6834,.F.);
#8792=ORIENTED_EDGE('',*,*,#6836,.F.);
#8793=ORIENTED_EDGE('',*,*,#6837,.F.);
#8794=ORIENTED_EDGE('',*,*,#6838,.F.);
#8795=ORIENTED_EDGE('',*,*,#6839,.T.);
#8796=ORIENTED_EDGE('',*,*,#6840,.F.);
#8797=ORIENTED_EDGE('',*,*,#6839,.F.);
#8798=ORIENTED_EDGE('',*,*,#6841,.F.);
#8799=ORIENTED_EDGE('',*,*,#6842,.T.);
#8800=ORIENTED_EDGE('',*,*,#6843,.F.);
#8801=ORIENTED_EDGE('',*,*,#6842,.F.);
#8802=ORIENTED_EDGE('',*,*,#6844,.F.);
#8803=ORIENTED_EDGE('',*,*,#6845,.T.);
#8804=ORIENTED_EDGE('',*,*,#6846,.F.);
#8805=ORIENTED_EDGE('',*,*,#6845,.F.);
#8806=ORIENTED_EDGE('',*,*,#6847,.F.);
#8807=ORIENTED_EDGE('',*,*,#6837,.T.);
#8808=ORIENTED_EDGE('',*,*,#6848,.F.);
#8809=ORIENTED_EDGE('',*,*,#6849,.F.);
#8810=ORIENTED_EDGE('',*,*,#6850,.F.);
#8811=ORIENTED_EDGE('',*,*,#6851,.T.);
#8812=ORIENTED_EDGE('',*,*,#6852,.F.);
#8813=ORIENTED_EDGE('',*,*,#6851,.F.);
#8814=ORIENTED_EDGE('',*,*,#6853,.F.);
#8815=ORIENTED_EDGE('',*,*,#6854,.T.);
#8816=ORIENTED_EDGE('',*,*,#6855,.F.);
#8817=ORIENTED_EDGE('',*,*,#6854,.F.);
#8818=ORIENTED_EDGE('',*,*,#6856,.F.);
#8819=ORIENTED_EDGE('',*,*,#6857,.T.);
#8820=ORIENTED_EDGE('',*,*,#6858,.F.);
#8821=ORIENTED_EDGE('',*,*,#6857,.F.);
#8822=ORIENTED_EDGE('',*,*,#6859,.F.);
#8823=ORIENTED_EDGE('',*,*,#6849,.T.);
#8824=ORIENTED_EDGE('',*,*,#6860,.F.);
#8825=ORIENTED_EDGE('',*,*,#6861,.T.);
#8826=ORIENTED_EDGE('',*,*,#6862,.F.);
#8827=ORIENTED_EDGE('',*,*,#6861,.F.);
#8828=ORIENTED_EDGE('',*,*,#6863,.F.);
#8829=ORIENTED_EDGE('',*,*,#6864,.T.);
#8830=ORIENTED_EDGE('',*,*,#6865,.F.);
#8831=ORIENTED_EDGE('',*,*,#6864,.F.);
#8832=ORIENTED_EDGE('',*,*,#6866,.F.);
#8833=ORIENTED_EDGE('',*,*,#6867,.F.);
#8834=ORIENTED_EDGE('',*,*,#6868,.F.);
#8835=ORIENTED_EDGE('',*,*,#6869,.T.);
#8836=ORIENTED_EDGE('',*,*,#6870,.F.);
#8837=ORIENTED_EDGE('',*,*,#6869,.F.);
#8838=ORIENTED_EDGE('',*,*,#6871,.F.);
#8839=ORIENTED_EDGE('',*,*,#6872,.T.);
#8840=ORIENTED_EDGE('',*,*,#6873,.F.);
#8841=ORIENTED_EDGE('',*,*,#6872,.F.);
#8842=ORIENTED_EDGE('',*,*,#6874,.F.);
#8843=ORIENTED_EDGE('',*,*,#6875,.T.);
#8844=ORIENTED_EDGE('',*,*,#6876,.F.);
#8845=ORIENTED_EDGE('',*,*,#6875,.F.);
#8846=ORIENTED_EDGE('',*,*,#6877,.F.);
#8847=ORIENTED_EDGE('',*,*,#6867,.T.);
#8848=ORIENTED_EDGE('',*,*,#6878,.F.);
#8849=ORIENTED_EDGE('',*,*,#6879,.F.);
#8850=ORIENTED_EDGE('',*,*,#6880,.F.);
#8851=ORIENTED_EDGE('',*,*,#6881,.T.);
#8852=ORIENTED_EDGE('',*,*,#6882,.F.);
#8853=ORIENTED_EDGE('',*,*,#6881,.F.);
#8854=ORIENTED_EDGE('',*,*,#6883,.F.);
#8855=ORIENTED_EDGE('',*,*,#6884,.T.);
#8856=ORIENTED_EDGE('',*,*,#6885,.F.);
#8857=ORIENTED_EDGE('',*,*,#6884,.F.);
#8858=ORIENTED_EDGE('',*,*,#6886,.F.);
#8859=ORIENTED_EDGE('',*,*,#6887,.T.);
#8860=ORIENTED_EDGE('',*,*,#6888,.F.);
#8861=ORIENTED_EDGE('',*,*,#6887,.F.);
#8862=ORIENTED_EDGE('',*,*,#6889,.F.);
#8863=ORIENTED_EDGE('',*,*,#6879,.T.);
#8864=ORIENTED_EDGE('',*,*,#6890,.F.);
#8865=ORIENTED_EDGE('',*,*,#6891,.T.);
#8866=ORIENTED_EDGE('',*,*,#6892,.F.);
#8867=ORIENTED_EDGE('',*,*,#6891,.F.);
#8868=ORIENTED_EDGE('',*,*,#6893,.F.);
#8869=ORIENTED_EDGE('',*,*,#6894,.T.);
#8870=ORIENTED_EDGE('',*,*,#6895,.F.);
#8871=ORIENTED_EDGE('',*,*,#6894,.F.);
#8872=ORIENTED_EDGE('',*,*,#6896,.F.);
#8873=ORIENTED_EDGE('',*,*,#6897,.T.);
#8874=ORIENTED_EDGE('',*,*,#6898,.F.);
#8875=ORIENTED_EDGE('',*,*,#6897,.F.);
#8876=ORIENTED_EDGE('',*,*,#6899,.T.);
#8877=ORIENTED_EDGE('',*,*,#6900,.T.);
#8878=ORIENTED_EDGE('',*,*,#6901,.T.);
#8879=ORIENTED_EDGE('',*,*,#6902,.T.);
#8880=ORIENTED_EDGE('',*,*,#6900,.F.);
#8881=ORIENTED_EDGE('',*,*,#6903,.T.);
#8882=ORIENTED_EDGE('',*,*,#6904,.F.);
#8883=ORIENTED_EDGE('',*,*,#6905,.F.);
#8884=ORIENTED_EDGE('',*,*,#6862,.T.);
#8885=ORIENTED_EDGE('',*,*,#6865,.T.);
#8886=ORIENTED_EDGE('',*,*,#6873,.T.);
#8887=ORIENTED_EDGE('',*,*,#6876,.T.);
#8888=ORIENTED_EDGE('',*,*,#6866,.T.);
#8889=ORIENTED_EDGE('',*,*,#6870,.T.);
#8890=ORIENTED_EDGE('',*,*,#6885,.T.);
#8891=ORIENTED_EDGE('',*,*,#6888,.T.);
#8892=ORIENTED_EDGE('',*,*,#6878,.T.);
#8893=ORIENTED_EDGE('',*,*,#6882,.T.);
#8894=ORIENTED_EDGE('',*,*,#6892,.T.);
#8895=ORIENTED_EDGE('',*,*,#6895,.T.);
#8896=ORIENTED_EDGE('',*,*,#6898,.T.);
#8897=ORIENTED_EDGE('',*,*,#6855,.T.);
#8898=ORIENTED_EDGE('',*,*,#6858,.T.);
#8899=ORIENTED_EDGE('',*,*,#6848,.T.);
#8900=ORIENTED_EDGE('',*,*,#6852,.T.);
#8901=ORIENTED_EDGE('',*,*,#6843,.T.);
#8902=ORIENTED_EDGE('',*,*,#6846,.T.);
#8903=ORIENTED_EDGE('',*,*,#6836,.T.);
#8904=ORIENTED_EDGE('',*,*,#6840,.T.);
#8905=ORIENTED_EDGE('',*,*,#6835,.T.);
#8906=ORIENTED_EDGE('',*,*,#6832,.T.);
#8907=ORIENTED_EDGE('',*,*,#6829,.T.);
#8908=ORIENTED_EDGE('',*,*,#6826,.T.);
#8909=ORIENTED_EDGE('',*,*,#6823,.T.);
#8910=ORIENTED_EDGE('',*,*,#6816,.T.);
#8911=ORIENTED_EDGE('',*,*,#6819,.T.);
#8912=ORIENTED_EDGE('',*,*,#6809,.T.);
#8913=ORIENTED_EDGE('',*,*,#6813,.T.);
#8914=ORIENTED_EDGE('',*,*,#6804,.T.);
#8915=ORIENTED_EDGE('',*,*,#6807,.T.);
#8916=ORIENTED_EDGE('',*,*,#6797,.T.);
#8917=ORIENTED_EDGE('',*,*,#6801,.T.);
#8918=ORIENTED_EDGE('',*,*,#6796,.T.);
#8919=ORIENTED_EDGE('',*,*,#6793,.T.);
#8920=ORIENTED_EDGE('',*,*,#6790,.T.);
#8921=ORIENTED_EDGE('',*,*,#6787,.T.);
#8922=ORIENTED_EDGE('',*,*,#6784,.T.);
#8923=ORIENTED_EDGE('',*,*,#6777,.T.);
#8924=ORIENTED_EDGE('',*,*,#6780,.T.);
#8925=ORIENTED_EDGE('',*,*,#6770,.T.);
#8926=ORIENTED_EDGE('',*,*,#6774,.T.);
#8927=ORIENTED_EDGE('',*,*,#6765,.T.);
#8928=ORIENTED_EDGE('',*,*,#6768,.T.);
#8929=ORIENTED_EDGE('',*,*,#6758,.T.);
#8930=ORIENTED_EDGE('',*,*,#6762,.T.);
#8931=ORIENTED_EDGE('',*,*,#6757,.T.);
#8932=ORIENTED_EDGE('',*,*,#6754,.T.);
#8933=ORIENTED_EDGE('',*,*,#6751,.T.);
#8934=ORIENTED_EDGE('',*,*,#6748,.T.);
#8935=ORIENTED_EDGE('',*,*,#6745,.T.);
#8936=ORIENTED_EDGE('',*,*,#6738,.T.);
#8937=ORIENTED_EDGE('',*,*,#6741,.T.);
#8938=ORIENTED_EDGE('',*,*,#6731,.T.);
#8939=ORIENTED_EDGE('',*,*,#6735,.T.);
#8940=ORIENTED_EDGE('',*,*,#6726,.T.);
#8941=ORIENTED_EDGE('',*,*,#6729,.T.);
#8942=ORIENTED_EDGE('',*,*,#6719,.T.);
#8943=ORIENTED_EDGE('',*,*,#6723,.T.);
#8944=ORIENTED_EDGE('',*,*,#6718,.T.);
#8945=ORIENTED_EDGE('',*,*,#6715,.T.);
#8946=ORIENTED_EDGE('',*,*,#6712,.T.);
#8947=ORIENTED_EDGE('',*,*,#6709,.T.);
#8948=ORIENTED_EDGE('',*,*,#6706,.T.);
#8949=ORIENTED_EDGE('',*,*,#6699,.T.);
#8950=ORIENTED_EDGE('',*,*,#6702,.T.);
#8951=ORIENTED_EDGE('',*,*,#6692,.T.);
#8952=ORIENTED_EDGE('',*,*,#6696,.T.);
#8953=ORIENTED_EDGE('',*,*,#6687,.T.);
#8954=ORIENTED_EDGE('',*,*,#6690,.T.);
#8955=ORIENTED_EDGE('',*,*,#6680,.T.);
#8956=ORIENTED_EDGE('',*,*,#6684,.T.);
#8957=ORIENTED_EDGE('',*,*,#6679,.T.);
#8958=ORIENTED_EDGE('',*,*,#6676,.T.);
#8959=ORIENTED_EDGE('',*,*,#6673,.T.);
#8960=ORIENTED_EDGE('',*,*,#6670,.T.);
#8961=ORIENTED_EDGE('',*,*,#6667,.T.);
#8962=ORIENTED_EDGE('',*,*,#6660,.T.);
#8963=ORIENTED_EDGE('',*,*,#6663,.T.);
#8964=ORIENTED_EDGE('',*,*,#6653,.T.);
#8965=ORIENTED_EDGE('',*,*,#6657,.T.);
#8966=ORIENTED_EDGE('',*,*,#6648,.T.);
#8967=ORIENTED_EDGE('',*,*,#6651,.T.);
#8968=ORIENTED_EDGE('',*,*,#6641,.T.);
#8969=ORIENTED_EDGE('',*,*,#6645,.T.);
#8970=ORIENTED_EDGE('',*,*,#6640,.T.);
#8971=ORIENTED_EDGE('',*,*,#6637,.T.);
#8972=ORIENTED_EDGE('',*,*,#6634,.T.);
#8973=ORIENTED_EDGE('',*,*,#6631,.T.);
#8974=ORIENTED_EDGE('',*,*,#6628,.T.);
#8975=ORIENTED_EDGE('',*,*,#6621,.T.);
#8976=ORIENTED_EDGE('',*,*,#6624,.T.);
#8977=ORIENTED_EDGE('',*,*,#6614,.T.);
#8978=ORIENTED_EDGE('',*,*,#6618,.T.);
#8979=ORIENTED_EDGE('',*,*,#6609,.T.);
#8980=ORIENTED_EDGE('',*,*,#6612,.T.);
#8981=ORIENTED_EDGE('',*,*,#6602,.T.);
#8982=ORIENTED_EDGE('',*,*,#6606,.T.);
#8983=ORIENTED_EDGE('',*,*,#6601,.T.);
#8984=ORIENTED_EDGE('',*,*,#6598,.T.);
#8985=ORIENTED_EDGE('',*,*,#6595,.T.);
#8986=ORIENTED_EDGE('',*,*,#6592,.T.);
#8987=ORIENTED_EDGE('',*,*,#6589,.T.);
#8988=ORIENTED_EDGE('',*,*,#6582,.T.);
#8989=ORIENTED_EDGE('',*,*,#6585,.T.);
#8990=ORIENTED_EDGE('',*,*,#6575,.T.);
#8991=ORIENTED_EDGE('',*,*,#6579,.T.);
#8992=ORIENTED_EDGE('',*,*,#6570,.T.);
#8993=ORIENTED_EDGE('',*,*,#6573,.T.);
#8994=ORIENTED_EDGE('',*,*,#6563,.T.);
#8995=ORIENTED_EDGE('',*,*,#6567,.T.);
#8996=ORIENTED_EDGE('',*,*,#6562,.T.);
#8997=ORIENTED_EDGE('',*,*,#6559,.T.);
#8998=ORIENTED_EDGE('',*,*,#6556,.T.);
#8999=ORIENTED_EDGE('',*,*,#6553,.T.);
#9000=ORIENTED_EDGE('',*,*,#6550,.T.);
#9001=ORIENTED_EDGE('',*,*,#6543,.T.);
#9002=ORIENTED_EDGE('',*,*,#6546,.T.);
#9003=ORIENTED_EDGE('',*,*,#6536,.T.);
#9004=ORIENTED_EDGE('',*,*,#6540,.T.);
#9005=ORIENTED_EDGE('',*,*,#6531,.T.);
#9006=ORIENTED_EDGE('',*,*,#6534,.T.);
#9007=ORIENTED_EDGE('',*,*,#6524,.T.);
#9008=ORIENTED_EDGE('',*,*,#6528,.T.);
#9009=ORIENTED_EDGE('',*,*,#6523,.T.);
#9010=ORIENTED_EDGE('',*,*,#6520,.T.);
#9011=ORIENTED_EDGE('',*,*,#6517,.T.);
#9012=ORIENTED_EDGE('',*,*,#6514,.T.);
#9013=ORIENTED_EDGE('',*,*,#6511,.T.);
#9014=ORIENTED_EDGE('',*,*,#6906,.T.);
#9015=ORIENTED_EDGE('',*,*,#6907,.T.);
#9016=ORIENTED_EDGE('',*,*,#6908,.T.);
#9017=ORIENTED_EDGE('',*,*,#6904,.T.);
#9018=ORIENTED_EDGE('',*,*,#6907,.F.);
#9019=ORIENTED_EDGE('',*,*,#6909,.T.);
#9020=ORIENTED_EDGE('',*,*,#6910,.T.);
#9021=ORIENTED_EDGE('',*,*,#6911,.T.);
#9022=ORIENTED_EDGE('',*,*,#6912,.F.);
#9023=ORIENTED_EDGE('',*,*,#6913,.F.);
#9024=ORIENTED_EDGE('',*,*,#6914,.F.);
#9025=ORIENTED_EDGE('',*,*,#6915,.F.);
#9026=ORIENTED_EDGE('',*,*,#6916,.F.);
#9027=ORIENTED_EDGE('',*,*,#6917,.F.);
#9028=ORIENTED_EDGE('',*,*,#6918,.F.);
#9029=ORIENTED_EDGE('',*,*,#6919,.F.);
#9030=ORIENTED_EDGE('',*,*,#6920,.F.);
#9031=ORIENTED_EDGE('',*,*,#6921,.F.);
#9032=ORIENTED_EDGE('',*,*,#6922,.F.);
#9033=ORIENTED_EDGE('',*,*,#6923,.F.);
#9034=ORIENTED_EDGE('',*,*,#6924,.F.);
#9035=ORIENTED_EDGE('',*,*,#6925,.F.);
#9036=ORIENTED_EDGE('',*,*,#6926,.F.);
#9037=ORIENTED_EDGE('',*,*,#6927,.F.);
#9038=ORIENTED_EDGE('',*,*,#6928,.F.);
#9039=ORIENTED_EDGE('',*,*,#6929,.F.);
#9040=ORIENTED_EDGE('',*,*,#6930,.F.);
#9041=ORIENTED_EDGE('',*,*,#6931,.F.);
#9042=ORIENTED_EDGE('',*,*,#6932,.F.);
#9043=ORIENTED_EDGE('',*,*,#6933,.F.);
#9044=ORIENTED_EDGE('',*,*,#6934,.F.);
#9045=ORIENTED_EDGE('',*,*,#6935,.F.);
#9046=ORIENTED_EDGE('',*,*,#6936,.F.);
#9047=ORIENTED_EDGE('',*,*,#6937,.F.);
#9048=ORIENTED_EDGE('',*,*,#6938,.F.);
#9049=ORIENTED_EDGE('',*,*,#6939,.F.);
#9050=ORIENTED_EDGE('',*,*,#6940,.F.);
#9051=ORIENTED_EDGE('',*,*,#6941,.F.);
#9052=ORIENTED_EDGE('',*,*,#6942,.F.);
#9053=ORIENTED_EDGE('',*,*,#6943,.F.);
#9054=ORIENTED_EDGE('',*,*,#6944,.F.);
#9055=ORIENTED_EDGE('',*,*,#6945,.F.);
#9056=ORIENTED_EDGE('',*,*,#6946,.F.);
#9057=ORIENTED_EDGE('',*,*,#6947,.F.);
#9058=ORIENTED_EDGE('',*,*,#6948,.F.);
#9059=ORIENTED_EDGE('',*,*,#6949,.F.);
#9060=ORIENTED_EDGE('',*,*,#6950,.F.);
#9061=ORIENTED_EDGE('',*,*,#6951,.F.);
#9062=ORIENTED_EDGE('',*,*,#6952,.F.);
#9063=ORIENTED_EDGE('',*,*,#6953,.F.);
#9064=ORIENTED_EDGE('',*,*,#6954,.F.);
#9065=ORIENTED_EDGE('',*,*,#6955,.F.);
#9066=ORIENTED_EDGE('',*,*,#6956,.F.);
#9067=ORIENTED_EDGE('',*,*,#6957,.F.);
#9068=ORIENTED_EDGE('',*,*,#6958,.F.);
#9069=ORIENTED_EDGE('',*,*,#6959,.T.);
#9070=ORIENTED_EDGE('',*,*,#6960,.T.);
#9071=ORIENTED_EDGE('',*,*,#6961,.T.);
#9072=ORIENTED_EDGE('',*,*,#6962,.T.);
#9073=ORIENTED_EDGE('',*,*,#6962,.F.);
#9074=ORIENTED_EDGE('',*,*,#6963,.F.);
#9075=ORIENTED_EDGE('',*,*,#6964,.F.);
#9076=ORIENTED_EDGE('',*,*,#6965,.T.);
#9077=ORIENTED_EDGE('',*,*,#6860,.T.);
#9078=ORIENTED_EDGE('',*,*,#6863,.T.);
#9079=ORIENTED_EDGE('',*,*,#6874,.T.);
#9080=ORIENTED_EDGE('',*,*,#6871,.T.);
#9081=ORIENTED_EDGE('',*,*,#6868,.T.);
#9082=ORIENTED_EDGE('',*,*,#6877,.T.);
#9083=ORIENTED_EDGE('',*,*,#6886,.T.);
#9084=ORIENTED_EDGE('',*,*,#6883,.T.);
#9085=ORIENTED_EDGE('',*,*,#6880,.T.);
#9086=ORIENTED_EDGE('',*,*,#6889,.T.);
#9087=ORIENTED_EDGE('',*,*,#6890,.T.);
#9088=ORIENTED_EDGE('',*,*,#6893,.T.);
#9089=ORIENTED_EDGE('',*,*,#6896,.T.);
#9090=ORIENTED_EDGE('',*,*,#6856,.T.);
#9091=ORIENTED_EDGE('',*,*,#6853,.T.);
#9092=ORIENTED_EDGE('',*,*,#6850,.T.);
#9093=ORIENTED_EDGE('',*,*,#6859,.T.);
#9094=ORIENTED_EDGE('',*,*,#6844,.T.);
#9095=ORIENTED_EDGE('',*,*,#6841,.T.);
#9096=ORIENTED_EDGE('',*,*,#6838,.T.);
#9097=ORIENTED_EDGE('',*,*,#6847,.T.);
#9098=ORIENTED_EDGE('',*,*,#6833,.T.);
#9099=ORIENTED_EDGE('',*,*,#6830,.T.);
#9100=ORIENTED_EDGE('',*,*,#6827,.T.);
#9101=ORIENTED_EDGE('',*,*,#6824,.T.);
#9102=ORIENTED_EDGE('',*,*,#6821,.T.);
#9103=ORIENTED_EDGE('',*,*,#6817,.T.);
#9104=ORIENTED_EDGE('',*,*,#6814,.T.);
#9105=ORIENTED_EDGE('',*,*,#6811,.T.);
#9106=ORIENTED_EDGE('',*,*,#6820,.T.);
#9107=ORIENTED_EDGE('',*,*,#6805,.T.);
#9108=ORIENTED_EDGE('',*,*,#6802,.T.);
#9109=ORIENTED_EDGE('',*,*,#6799,.T.);
#9110=ORIENTED_EDGE('',*,*,#6808,.T.);
#9111=ORIENTED_EDGE('',*,*,#6794,.T.);
#9112=ORIENTED_EDGE('',*,*,#6791,.T.);
#9113=ORIENTED_EDGE('',*,*,#6788,.T.);
#9114=ORIENTED_EDGE('',*,*,#6785,.T.);
#9115=ORIENTED_EDGE('',*,*,#6782,.T.);
#9116=ORIENTED_EDGE('',*,*,#6778,.T.);
#9117=ORIENTED_EDGE('',*,*,#6775,.T.);
#9118=ORIENTED_EDGE('',*,*,#6772,.T.);
#9119=ORIENTED_EDGE('',*,*,#6781,.T.);
#9120=ORIENTED_EDGE('',*,*,#6766,.T.);
#9121=ORIENTED_EDGE('',*,*,#6763,.T.);
#9122=ORIENTED_EDGE('',*,*,#6760,.T.);
#9123=ORIENTED_EDGE('',*,*,#6769,.T.);
#9124=ORIENTED_EDGE('',*,*,#6755,.T.);
#9125=ORIENTED_EDGE('',*,*,#6752,.T.);
#9126=ORIENTED_EDGE('',*,*,#6749,.T.);
#9127=ORIENTED_EDGE('',*,*,#6746,.T.);
#9128=ORIENTED_EDGE('',*,*,#6743,.T.);
#9129=ORIENTED_EDGE('',*,*,#6739,.T.);
#9130=ORIENTED_EDGE('',*,*,#6736,.T.);
#9131=ORIENTED_EDGE('',*,*,#6733,.T.);
#9132=ORIENTED_EDGE('',*,*,#6742,.T.);
#9133=ORIENTED_EDGE('',*,*,#6727,.T.);
#9134=ORIENTED_EDGE('',*,*,#6724,.T.);
#9135=ORIENTED_EDGE('',*,*,#6721,.T.);
#9136=ORIENTED_EDGE('',*,*,#6730,.T.);
#9137=ORIENTED_EDGE('',*,*,#6716,.T.);
#9138=ORIENTED_EDGE('',*,*,#6713,.T.);
#9139=ORIENTED_EDGE('',*,*,#6710,.T.);
#9140=ORIENTED_EDGE('',*,*,#6707,.T.);
#9141=ORIENTED_EDGE('',*,*,#6704,.T.);
#9142=ORIENTED_EDGE('',*,*,#6700,.T.);
#9143=ORIENTED_EDGE('',*,*,#6697,.T.);
#9144=ORIENTED_EDGE('',*,*,#6694,.T.);
#9145=ORIENTED_EDGE('',*,*,#6703,.T.);
#9146=ORIENTED_EDGE('',*,*,#6688,.T.);
#9147=ORIENTED_EDGE('',*,*,#6685,.T.);
#9148=ORIENTED_EDGE('',*,*,#6682,.T.);
#9149=ORIENTED_EDGE('',*,*,#6691,.T.);
#9150=ORIENTED_EDGE('',*,*,#6677,.T.);
#9151=ORIENTED_EDGE('',*,*,#6674,.T.);
#9152=ORIENTED_EDGE('',*,*,#6671,.T.);
#9153=ORIENTED_EDGE('',*,*,#6668,.T.);
#9154=ORIENTED_EDGE('',*,*,#6665,.T.);
#9155=ORIENTED_EDGE('',*,*,#6661,.T.);
#9156=ORIENTED_EDGE('',*,*,#6658,.T.);
#9157=ORIENTED_EDGE('',*,*,#6655,.T.);
#9158=ORIENTED_EDGE('',*,*,#6664,.T.);
#9159=ORIENTED_EDGE('',*,*,#6649,.T.);
#9160=ORIENTED_EDGE('',*,*,#6646,.T.);
#9161=ORIENTED_EDGE('',*,*,#6643,.T.);
#9162=ORIENTED_EDGE('',*,*,#6652,.T.);
#9163=ORIENTED_EDGE('',*,*,#6638,.T.);
#9164=ORIENTED_EDGE('',*,*,#6635,.T.);
#9165=ORIENTED_EDGE('',*,*,#6632,.T.);
#9166=ORIENTED_EDGE('',*,*,#6629,.T.);
#9167=ORIENTED_EDGE('',*,*,#6626,.T.);
#9168=ORIENTED_EDGE('',*,*,#6622,.T.);
#9169=ORIENTED_EDGE('',*,*,#6619,.T.);
#9170=ORIENTED_EDGE('',*,*,#6616,.T.);
#9171=ORIENTED_EDGE('',*,*,#6625,.T.);
#9172=ORIENTED_EDGE('',*,*,#6610,.T.);
#9173=ORIENTED_EDGE('',*,*,#6607,.T.);
#9174=ORIENTED_EDGE('',*,*,#6604,.T.);
#9175=ORIENTED_EDGE('',*,*,#6613,.T.);
#9176=ORIENTED_EDGE('',*,*,#6599,.T.);
#9177=ORIENTED_EDGE('',*,*,#6596,.T.);
#9178=ORIENTED_EDGE('',*,*,#6593,.T.);
#9179=ORIENTED_EDGE('',*,*,#6590,.T.);
#9180=ORIENTED_EDGE('',*,*,#6587,.T.);
#9181=ORIENTED_EDGE('',*,*,#6583,.T.);
#9182=ORIENTED_EDGE('',*,*,#6580,.T.);
#9183=ORIENTED_EDGE('',*,*,#6577,.T.);
#9184=ORIENTED_EDGE('',*,*,#6586,.T.);
#9185=ORIENTED_EDGE('',*,*,#6571,.T.);
#9186=ORIENTED_EDGE('',*,*,#6568,.T.);
#9187=ORIENTED_EDGE('',*,*,#6565,.T.);
#9188=ORIENTED_EDGE('',*,*,#6574,.T.);
#9189=ORIENTED_EDGE('',*,*,#6560,.T.);
#9190=ORIENTED_EDGE('',*,*,#6557,.T.);
#9191=ORIENTED_EDGE('',*,*,#6554,.T.);
#9192=ORIENTED_EDGE('',*,*,#6551,.T.);
#9193=ORIENTED_EDGE('',*,*,#6548,.T.);
#9194=ORIENTED_EDGE('',*,*,#6544,.T.);
#9195=ORIENTED_EDGE('',*,*,#6541,.T.);
#9196=ORIENTED_EDGE('',*,*,#6538,.T.);
#9197=ORIENTED_EDGE('',*,*,#6547,.T.);
#9198=ORIENTED_EDGE('',*,*,#6532,.T.);
#9199=ORIENTED_EDGE('',*,*,#6529,.T.);
#9200=ORIENTED_EDGE('',*,*,#6526,.T.);
#9201=ORIENTED_EDGE('',*,*,#6535,.T.);
#9202=ORIENTED_EDGE('',*,*,#6521,.T.);
#9203=ORIENTED_EDGE('',*,*,#6518,.T.);
#9204=ORIENTED_EDGE('',*,*,#6515,.T.);
#9205=ORIENTED_EDGE('',*,*,#6512,.T.);
#9206=ORIENTED_EDGE('',*,*,#6509,.T.);
#9207=ORIENTED_EDGE('',*,*,#6961,.F.);
#9208=ORIENTED_EDGE('',*,*,#6966,.F.);
#9209=ORIENTED_EDGE('',*,*,#6967,.F.);
#9210=ORIENTED_EDGE('',*,*,#6909,.F.);
#9211=ORIENTED_EDGE('',*,*,#6906,.F.);
#9212=ORIENTED_EDGE('',*,*,#6903,.F.);
#9213=ORIENTED_EDGE('',*,*,#6899,.F.);
#9214=ORIENTED_EDGE('',*,*,#6968,.F.);
#9215=ORIENTED_EDGE('',*,*,#6969,.F.);
#9216=ORIENTED_EDGE('',*,*,#6970,.F.);
#9217=ORIENTED_EDGE('',*,*,#6971,.F.);
#9218=ORIENTED_EDGE('',*,*,#6963,.T.);
#9219=ORIENTED_EDGE('',*,*,#6972,.T.);
#9220=ORIENTED_EDGE('',*,*,#6964,.T.);
#9221=ORIENTED_EDGE('',*,*,#6971,.T.);
#9222=ORIENTED_EDGE('',*,*,#6973,.T.);
#9223=ORIENTED_EDGE('',*,*,#6974,.F.);
#9224=ORIENTED_EDGE('',*,*,#6975,.T.);
#9225=ORIENTED_EDGE('',*,*,#6912,.T.);
#9226=ORIENTED_EDGE('',*,*,#6975,.F.);
#9227=ORIENTED_EDGE('',*,*,#6976,.F.);
#9228=ORIENTED_EDGE('',*,*,#6977,.T.);
#9229=ORIENTED_EDGE('',*,*,#6913,.T.);
#9230=ORIENTED_EDGE('',*,*,#6977,.F.);
#9231=ORIENTED_EDGE('',*,*,#6978,.F.);
#9232=ORIENTED_EDGE('',*,*,#6979,.T.);
#9233=ORIENTED_EDGE('',*,*,#6914,.T.);
#9234=ORIENTED_EDGE('',*,*,#6979,.F.);
#9235=ORIENTED_EDGE('',*,*,#6980,.F.);
#9236=ORIENTED_EDGE('',*,*,#6981,.T.);
#9237=ORIENTED_EDGE('',*,*,#6915,.T.);
#9238=ORIENTED_EDGE('',*,*,#6981,.F.);
#9239=ORIENTED_EDGE('',*,*,#6982,.F.);
#9240=ORIENTED_EDGE('',*,*,#6983,.T.);
#9241=ORIENTED_EDGE('',*,*,#6916,.T.);
#9242=ORIENTED_EDGE('',*,*,#6983,.F.);
#9243=ORIENTED_EDGE('',*,*,#6984,.F.);
#9244=ORIENTED_EDGE('',*,*,#6985,.T.);
#9245=ORIENTED_EDGE('',*,*,#6917,.T.);
#9246=ORIENTED_EDGE('',*,*,#6985,.F.);
#9247=ORIENTED_EDGE('',*,*,#6986,.F.);
#9248=ORIENTED_EDGE('',*,*,#6987,.T.);
#9249=ORIENTED_EDGE('',*,*,#6918,.T.);
#9250=ORIENTED_EDGE('',*,*,#6987,.F.);
#9251=ORIENTED_EDGE('',*,*,#6988,.F.);
#9252=ORIENTED_EDGE('',*,*,#6989,.T.);
#9253=ORIENTED_EDGE('',*,*,#6919,.T.);
#9254=ORIENTED_EDGE('',*,*,#6989,.F.);
#9255=ORIENTED_EDGE('',*,*,#6990,.F.);
#9256=ORIENTED_EDGE('',*,*,#6991,.T.);
#9257=ORIENTED_EDGE('',*,*,#6920,.T.);
#9258=ORIENTED_EDGE('',*,*,#6991,.F.);
#9259=ORIENTED_EDGE('',*,*,#6992,.F.);
#9260=ORIENTED_EDGE('',*,*,#6993,.T.);
#9261=ORIENTED_EDGE('',*,*,#6921,.T.);
#9262=ORIENTED_EDGE('',*,*,#6993,.F.);
#9263=ORIENTED_EDGE('',*,*,#6994,.F.);
#9264=ORIENTED_EDGE('',*,*,#6995,.T.);
#9265=ORIENTED_EDGE('',*,*,#6922,.T.);
#9266=ORIENTED_EDGE('',*,*,#6995,.F.);
#9267=ORIENTED_EDGE('',*,*,#6996,.F.);
#9268=ORIENTED_EDGE('',*,*,#6997,.T.);
#9269=ORIENTED_EDGE('',*,*,#6923,.T.);
#9270=ORIENTED_EDGE('',*,*,#6997,.F.);
#9271=ORIENTED_EDGE('',*,*,#6998,.F.);
#9272=ORIENTED_EDGE('',*,*,#6999,.T.);
#9273=ORIENTED_EDGE('',*,*,#6924,.T.);
#9274=ORIENTED_EDGE('',*,*,#6999,.F.);
#9275=ORIENTED_EDGE('',*,*,#7000,.F.);
#9276=ORIENTED_EDGE('',*,*,#7001,.T.);
#9277=ORIENTED_EDGE('',*,*,#6925,.T.);
#9278=ORIENTED_EDGE('',*,*,#7001,.F.);
#9279=ORIENTED_EDGE('',*,*,#7002,.F.);
#9280=ORIENTED_EDGE('',*,*,#7003,.T.);
#9281=ORIENTED_EDGE('',*,*,#6926,.T.);
#9282=ORIENTED_EDGE('',*,*,#7003,.F.);
#9283=ORIENTED_EDGE('',*,*,#7004,.F.);
#9284=ORIENTED_EDGE('',*,*,#7005,.T.);
#9285=ORIENTED_EDGE('',*,*,#6927,.T.);
#9286=ORIENTED_EDGE('',*,*,#7005,.F.);
#9287=ORIENTED_EDGE('',*,*,#7006,.F.);
#9288=ORIENTED_EDGE('',*,*,#7007,.T.);
#9289=ORIENTED_EDGE('',*,*,#6928,.T.);
#9290=ORIENTED_EDGE('',*,*,#7007,.F.);
#9291=ORIENTED_EDGE('',*,*,#7008,.F.);
#9292=ORIENTED_EDGE('',*,*,#7009,.T.);
#9293=ORIENTED_EDGE('',*,*,#6929,.T.);
#9294=ORIENTED_EDGE('',*,*,#7009,.F.);
#9295=ORIENTED_EDGE('',*,*,#7010,.F.);
#9296=ORIENTED_EDGE('',*,*,#7011,.T.);
#9297=ORIENTED_EDGE('',*,*,#6930,.T.);
#9298=ORIENTED_EDGE('',*,*,#7011,.F.);
#9299=ORIENTED_EDGE('',*,*,#7012,.F.);
#9300=ORIENTED_EDGE('',*,*,#7013,.T.);
#9301=ORIENTED_EDGE('',*,*,#6931,.T.);
#9302=ORIENTED_EDGE('',*,*,#7013,.F.);
#9303=ORIENTED_EDGE('',*,*,#7014,.F.);
#9304=ORIENTED_EDGE('',*,*,#7015,.T.);
#9305=ORIENTED_EDGE('',*,*,#6932,.T.);
#9306=ORIENTED_EDGE('',*,*,#7015,.F.);
#9307=ORIENTED_EDGE('',*,*,#7016,.F.);
#9308=ORIENTED_EDGE('',*,*,#7017,.T.);
#9309=ORIENTED_EDGE('',*,*,#6933,.T.);
#9310=ORIENTED_EDGE('',*,*,#7017,.F.);
#9311=ORIENTED_EDGE('',*,*,#7018,.F.);
#9312=ORIENTED_EDGE('',*,*,#7019,.T.);
#9313=ORIENTED_EDGE('',*,*,#6934,.T.);
#9314=ORIENTED_EDGE('',*,*,#7019,.F.);
#9315=ORIENTED_EDGE('',*,*,#7020,.F.);
#9316=ORIENTED_EDGE('',*,*,#7021,.T.);
#9317=ORIENTED_EDGE('',*,*,#6935,.T.);
#9318=ORIENTED_EDGE('',*,*,#7021,.F.);
#9319=ORIENTED_EDGE('',*,*,#7022,.F.);
#9320=ORIENTED_EDGE('',*,*,#7023,.T.);
#9321=ORIENTED_EDGE('',*,*,#6936,.T.);
#9322=ORIENTED_EDGE('',*,*,#7023,.F.);
#9323=ORIENTED_EDGE('',*,*,#7024,.F.);
#9324=ORIENTED_EDGE('',*,*,#7025,.T.);
#9325=ORIENTED_EDGE('',*,*,#6937,.T.);
#9326=ORIENTED_EDGE('',*,*,#7025,.F.);
#9327=ORIENTED_EDGE('',*,*,#7026,.F.);
#9328=ORIENTED_EDGE('',*,*,#7027,.T.);
#9329=ORIENTED_EDGE('',*,*,#6938,.T.);
#9330=ORIENTED_EDGE('',*,*,#7027,.F.);
#9331=ORIENTED_EDGE('',*,*,#7028,.F.);
#9332=ORIENTED_EDGE('',*,*,#7029,.T.);
#9333=ORIENTED_EDGE('',*,*,#6939,.T.);
#9334=ORIENTED_EDGE('',*,*,#7029,.F.);
#9335=ORIENTED_EDGE('',*,*,#7030,.F.);
#9336=ORIENTED_EDGE('',*,*,#7031,.T.);
#9337=ORIENTED_EDGE('',*,*,#6940,.T.);
#9338=ORIENTED_EDGE('',*,*,#7031,.F.);
#9339=ORIENTED_EDGE('',*,*,#7032,.F.);
#9340=ORIENTED_EDGE('',*,*,#7033,.T.);
#9341=ORIENTED_EDGE('',*,*,#6941,.T.);
#9342=ORIENTED_EDGE('',*,*,#7033,.F.);
#9343=ORIENTED_EDGE('',*,*,#7034,.F.);
#9344=ORIENTED_EDGE('',*,*,#7035,.T.);
#9345=ORIENTED_EDGE('',*,*,#6942,.T.);
#9346=ORIENTED_EDGE('',*,*,#7035,.F.);
#9347=ORIENTED_EDGE('',*,*,#7036,.F.);
#9348=ORIENTED_EDGE('',*,*,#7037,.T.);
#9349=ORIENTED_EDGE('',*,*,#6943,.T.);
#9350=ORIENTED_EDGE('',*,*,#7037,.F.);
#9351=ORIENTED_EDGE('',*,*,#7038,.F.);
#9352=ORIENTED_EDGE('',*,*,#7039,.T.);
#9353=ORIENTED_EDGE('',*,*,#6944,.T.);
#9354=ORIENTED_EDGE('',*,*,#7039,.F.);
#9355=ORIENTED_EDGE('',*,*,#7040,.F.);
#9356=ORIENTED_EDGE('',*,*,#7041,.T.);
#9357=ORIENTED_EDGE('',*,*,#6945,.T.);
#9358=ORIENTED_EDGE('',*,*,#7041,.F.);
#9359=ORIENTED_EDGE('',*,*,#7042,.F.);
#9360=ORIENTED_EDGE('',*,*,#7043,.T.);
#9361=ORIENTED_EDGE('',*,*,#6946,.T.);
#9362=ORIENTED_EDGE('',*,*,#7043,.F.);
#9363=ORIENTED_EDGE('',*,*,#7044,.F.);
#9364=ORIENTED_EDGE('',*,*,#7045,.T.);
#9365=ORIENTED_EDGE('',*,*,#6947,.T.);
#9366=ORIENTED_EDGE('',*,*,#7045,.F.);
#9367=ORIENTED_EDGE('',*,*,#7046,.F.);
#9368=ORIENTED_EDGE('',*,*,#7047,.T.);
#9369=ORIENTED_EDGE('',*,*,#6948,.T.);
#9370=ORIENTED_EDGE('',*,*,#7047,.F.);
#9371=ORIENTED_EDGE('',*,*,#7048,.F.);
#9372=ORIENTED_EDGE('',*,*,#7049,.T.);
#9373=ORIENTED_EDGE('',*,*,#6949,.T.);
#9374=ORIENTED_EDGE('',*,*,#7049,.F.);
#9375=ORIENTED_EDGE('',*,*,#7050,.F.);
#9376=ORIENTED_EDGE('',*,*,#7051,.T.);
#9377=ORIENTED_EDGE('',*,*,#6950,.T.);
#9378=ORIENTED_EDGE('',*,*,#7051,.F.);
#9379=ORIENTED_EDGE('',*,*,#7052,.F.);
#9380=ORIENTED_EDGE('',*,*,#7053,.T.);
#9381=ORIENTED_EDGE('',*,*,#6951,.T.);
#9382=ORIENTED_EDGE('',*,*,#7053,.F.);
#9383=ORIENTED_EDGE('',*,*,#7054,.F.);
#9384=ORIENTED_EDGE('',*,*,#7055,.T.);
#9385=ORIENTED_EDGE('',*,*,#6952,.T.);
#9386=ORIENTED_EDGE('',*,*,#7055,.F.);
#9387=ORIENTED_EDGE('',*,*,#7056,.F.);
#9388=ORIENTED_EDGE('',*,*,#7057,.T.);
#9389=ORIENTED_EDGE('',*,*,#6953,.T.);
#9390=ORIENTED_EDGE('',*,*,#7057,.F.);
#9391=ORIENTED_EDGE('',*,*,#7058,.F.);
#9392=ORIENTED_EDGE('',*,*,#7059,.T.);
#9393=ORIENTED_EDGE('',*,*,#6954,.T.);
#9394=ORIENTED_EDGE('',*,*,#7059,.F.);
#9395=ORIENTED_EDGE('',*,*,#7060,.F.);
#9396=ORIENTED_EDGE('',*,*,#7061,.T.);
#9397=ORIENTED_EDGE('',*,*,#6955,.T.);
#9398=ORIENTED_EDGE('',*,*,#7061,.F.);
#9399=ORIENTED_EDGE('',*,*,#7062,.F.);
#9400=ORIENTED_EDGE('',*,*,#7063,.T.);
#9401=ORIENTED_EDGE('',*,*,#6956,.T.);
#9402=ORIENTED_EDGE('',*,*,#7063,.F.);
#9403=ORIENTED_EDGE('',*,*,#7064,.F.);
#9404=ORIENTED_EDGE('',*,*,#7065,.T.);
#9405=ORIENTED_EDGE('',*,*,#6957,.T.);
#9406=ORIENTED_EDGE('',*,*,#7065,.F.);
#9407=ORIENTED_EDGE('',*,*,#7066,.F.);
#9408=ORIENTED_EDGE('',*,*,#7067,.T.);
#9409=ORIENTED_EDGE('',*,*,#6958,.T.);
#9410=ORIENTED_EDGE('',*,*,#7067,.F.);
#9411=ORIENTED_EDGE('',*,*,#6910,.F.);
#9412=ORIENTED_EDGE('',*,*,#6967,.T.);
#9413=ORIENTED_EDGE('',*,*,#7068,.F.);
#9414=ORIENTED_EDGE('',*,*,#7069,.F.);
#9415=ORIENTED_EDGE('',*,*,#6960,.F.);
#9416=ORIENTED_EDGE('',*,*,#7070,.T.);
#9417=ORIENTED_EDGE('',*,*,#7068,.T.);
#9418=ORIENTED_EDGE('',*,*,#6966,.T.);
#9419=ORIENTED_EDGE('',*,*,#6974,.T.);
#9420=ORIENTED_EDGE('',*,*,#6976,.T.);
#9421=ORIENTED_EDGE('',*,*,#6978,.T.);
#9422=ORIENTED_EDGE('',*,*,#6980,.T.);
#9423=ORIENTED_EDGE('',*,*,#6982,.T.);
#9424=ORIENTED_EDGE('',*,*,#6984,.T.);
#9425=ORIENTED_EDGE('',*,*,#6986,.T.);
#9426=ORIENTED_EDGE('',*,*,#6988,.T.);
#9427=ORIENTED_EDGE('',*,*,#6990,.T.);
#9428=ORIENTED_EDGE('',*,*,#6992,.T.);
#9429=ORIENTED_EDGE('',*,*,#6994,.T.);
#9430=ORIENTED_EDGE('',*,*,#6996,.T.);
#9431=ORIENTED_EDGE('',*,*,#6998,.T.);
#9432=ORIENTED_EDGE('',*,*,#7000,.T.);
#9433=ORIENTED_EDGE('',*,*,#7002,.T.);
#9434=ORIENTED_EDGE('',*,*,#7004,.T.);
#9435=ORIENTED_EDGE('',*,*,#7006,.T.);
#9436=ORIENTED_EDGE('',*,*,#7008,.T.);
#9437=ORIENTED_EDGE('',*,*,#7010,.T.);
#9438=ORIENTED_EDGE('',*,*,#7012,.T.);
#9439=ORIENTED_EDGE('',*,*,#7014,.T.);
#9440=ORIENTED_EDGE('',*,*,#7016,.T.);
#9441=ORIENTED_EDGE('',*,*,#7018,.T.);
#9442=ORIENTED_EDGE('',*,*,#7020,.T.);
#9443=ORIENTED_EDGE('',*,*,#7022,.T.);
#9444=ORIENTED_EDGE('',*,*,#7024,.T.);
#9445=ORIENTED_EDGE('',*,*,#7026,.T.);
#9446=ORIENTED_EDGE('',*,*,#7028,.T.);
#9447=ORIENTED_EDGE('',*,*,#7030,.T.);
#9448=ORIENTED_EDGE('',*,*,#7032,.T.);
#9449=ORIENTED_EDGE('',*,*,#7034,.T.);
#9450=ORIENTED_EDGE('',*,*,#7036,.T.);
#9451=ORIENTED_EDGE('',*,*,#7038,.T.);
#9452=ORIENTED_EDGE('',*,*,#7040,.T.);
#9453=ORIENTED_EDGE('',*,*,#7042,.T.);
#9454=ORIENTED_EDGE('',*,*,#7044,.T.);
#9455=ORIENTED_EDGE('',*,*,#7046,.T.);
#9456=ORIENTED_EDGE('',*,*,#7048,.T.);
#9457=ORIENTED_EDGE('',*,*,#7050,.T.);
#9458=ORIENTED_EDGE('',*,*,#7052,.T.);
#9459=ORIENTED_EDGE('',*,*,#7054,.T.);
#9460=ORIENTED_EDGE('',*,*,#7056,.T.);
#9461=ORIENTED_EDGE('',*,*,#7058,.T.);
#9462=ORIENTED_EDGE('',*,*,#7060,.T.);
#9463=ORIENTED_EDGE('',*,*,#7062,.T.);
#9464=ORIENTED_EDGE('',*,*,#7064,.T.);
#9465=ORIENTED_EDGE('',*,*,#7066,.T.);
#9466=ORIENTED_EDGE('',*,*,#7071,.F.);
#9467=ORIENTED_EDGE('',*,*,#7072,.T.);
#9468=ORIENTED_EDGE('',*,*,#7073,.T.);
#9469=ORIENTED_EDGE('',*,*,#7072,.F.);
#9470=ORIENTED_EDGE('',*,*,#7074,.F.);
#9471=ORIENTED_EDGE('',*,*,#7075,.T.);
#9472=ORIENTED_EDGE('',*,*,#7076,.T.);
#9473=ORIENTED_EDGE('',*,*,#7075,.F.);
#9474=ORIENTED_EDGE('',*,*,#7077,.F.);
#9475=ORIENTED_EDGE('',*,*,#7078,.T.);
#9476=ORIENTED_EDGE('',*,*,#7079,.T.);
#9477=ORIENTED_EDGE('',*,*,#7078,.F.);
#9478=ORIENTED_EDGE('',*,*,#7080,.F.);
#9479=ORIENTED_EDGE('',*,*,#7081,.T.);
#9480=ORIENTED_EDGE('',*,*,#7082,.T.);
#9481=ORIENTED_EDGE('',*,*,#7081,.F.);
#9482=ORIENTED_EDGE('',*,*,#7083,.F.);
#9483=ORIENTED_EDGE('',*,*,#7084,.T.);
#9484=ORIENTED_EDGE('',*,*,#7085,.T.);
#9485=ORIENTED_EDGE('',*,*,#7084,.F.);
#9486=ORIENTED_EDGE('',*,*,#7086,.F.);
#9487=ORIENTED_EDGE('',*,*,#7087,.T.);
#9488=ORIENTED_EDGE('',*,*,#7088,.T.);
#9489=ORIENTED_EDGE('',*,*,#7087,.F.);
#9490=ORIENTED_EDGE('',*,*,#7089,.F.);
#9491=ORIENTED_EDGE('',*,*,#7090,.T.);
#9492=ORIENTED_EDGE('',*,*,#7091,.T.);
#9493=ORIENTED_EDGE('',*,*,#7090,.F.);
#9494=ORIENTED_EDGE('',*,*,#7092,.F.);
#9495=ORIENTED_EDGE('',*,*,#7093,.T.);
#9496=ORIENTED_EDGE('',*,*,#7094,.T.);
#9497=ORIENTED_EDGE('',*,*,#7093,.F.);
#9498=ORIENTED_EDGE('',*,*,#7095,.F.);
#9499=ORIENTED_EDGE('',*,*,#7096,.T.);
#9500=ORIENTED_EDGE('',*,*,#7097,.T.);
#9501=ORIENTED_EDGE('',*,*,#7096,.F.);
#9502=ORIENTED_EDGE('',*,*,#7098,.F.);
#9503=ORIENTED_EDGE('',*,*,#7099,.T.);
#9504=ORIENTED_EDGE('',*,*,#7100,.T.);
#9505=ORIENTED_EDGE('',*,*,#7099,.F.);
#9506=ORIENTED_EDGE('',*,*,#7101,.F.);
#9507=ORIENTED_EDGE('',*,*,#7102,.T.);
#9508=ORIENTED_EDGE('',*,*,#7103,.T.);
#9509=ORIENTED_EDGE('',*,*,#7102,.F.);
#9510=ORIENTED_EDGE('',*,*,#7104,.F.);
#9511=ORIENTED_EDGE('',*,*,#7105,.T.);
#9512=ORIENTED_EDGE('',*,*,#7106,.T.);
#9513=ORIENTED_EDGE('',*,*,#7105,.F.);
#9514=ORIENTED_EDGE('',*,*,#7107,.F.);
#9515=ORIENTED_EDGE('',*,*,#7108,.T.);
#9516=ORIENTED_EDGE('',*,*,#7109,.T.);
#9517=ORIENTED_EDGE('',*,*,#7108,.F.);
#9518=ORIENTED_EDGE('',*,*,#7110,.F.);
#9519=ORIENTED_EDGE('',*,*,#7111,.T.);
#9520=ORIENTED_EDGE('',*,*,#7112,.T.);
#9521=ORIENTED_EDGE('',*,*,#7111,.F.);
#9522=ORIENTED_EDGE('',*,*,#7113,.F.);
#9523=ORIENTED_EDGE('',*,*,#7114,.T.);
#9524=ORIENTED_EDGE('',*,*,#7115,.T.);
#9525=ORIENTED_EDGE('',*,*,#7114,.F.);
#9526=ORIENTED_EDGE('',*,*,#7116,.F.);
#9527=ORIENTED_EDGE('',*,*,#7117,.T.);
#9528=ORIENTED_EDGE('',*,*,#7118,.T.);
#9529=ORIENTED_EDGE('',*,*,#7117,.F.);
#9530=ORIENTED_EDGE('',*,*,#7119,.F.);
#9531=ORIENTED_EDGE('',*,*,#7120,.T.);
#9532=ORIENTED_EDGE('',*,*,#7121,.T.);
#9533=ORIENTED_EDGE('',*,*,#7120,.F.);
#9534=ORIENTED_EDGE('',*,*,#7122,.F.);
#9535=ORIENTED_EDGE('',*,*,#7123,.T.);
#9536=ORIENTED_EDGE('',*,*,#7124,.T.);
#9537=ORIENTED_EDGE('',*,*,#7123,.F.);
#9538=ORIENTED_EDGE('',*,*,#7125,.F.);
#9539=ORIENTED_EDGE('',*,*,#7126,.T.);
#9540=ORIENTED_EDGE('',*,*,#7127,.T.);
#9541=ORIENTED_EDGE('',*,*,#7126,.F.);
#9542=ORIENTED_EDGE('',*,*,#7128,.F.);
#9543=ORIENTED_EDGE('',*,*,#7129,.T.);
#9544=ORIENTED_EDGE('',*,*,#7130,.T.);
#9545=ORIENTED_EDGE('',*,*,#7129,.F.);
#9546=ORIENTED_EDGE('',*,*,#7131,.F.);
#9547=ORIENTED_EDGE('',*,*,#7132,.T.);
#9548=ORIENTED_EDGE('',*,*,#7133,.T.);
#9549=ORIENTED_EDGE('',*,*,#7132,.F.);
#9550=ORIENTED_EDGE('',*,*,#7134,.F.);
#9551=ORIENTED_EDGE('',*,*,#7135,.T.);
#9552=ORIENTED_EDGE('',*,*,#7136,.T.);
#9553=ORIENTED_EDGE('',*,*,#7135,.F.);
#9554=ORIENTED_EDGE('',*,*,#7137,.F.);
#9555=ORIENTED_EDGE('',*,*,#7138,.T.);
#9556=ORIENTED_EDGE('',*,*,#7139,.T.);
#9557=ORIENTED_EDGE('',*,*,#7138,.F.);
#9558=ORIENTED_EDGE('',*,*,#7140,.F.);
#9559=ORIENTED_EDGE('',*,*,#7141,.T.);
#9560=ORIENTED_EDGE('',*,*,#7142,.T.);
#9561=ORIENTED_EDGE('',*,*,#7141,.F.);
#9562=ORIENTED_EDGE('',*,*,#7143,.F.);
#9563=ORIENTED_EDGE('',*,*,#7144,.T.);
#9564=ORIENTED_EDGE('',*,*,#7145,.T.);
#9565=ORIENTED_EDGE('',*,*,#7144,.F.);
#9566=ORIENTED_EDGE('',*,*,#7146,.F.);
#9567=ORIENTED_EDGE('',*,*,#7147,.T.);
#9568=ORIENTED_EDGE('',*,*,#7148,.T.);
#9569=ORIENTED_EDGE('',*,*,#7147,.F.);
#9570=ORIENTED_EDGE('',*,*,#7149,.F.);
#9571=ORIENTED_EDGE('',*,*,#7150,.T.);
#9572=ORIENTED_EDGE('',*,*,#7151,.T.);
#9573=ORIENTED_EDGE('',*,*,#7150,.F.);
#9574=ORIENTED_EDGE('',*,*,#7152,.F.);
#9575=ORIENTED_EDGE('',*,*,#7153,.T.);
#9576=ORIENTED_EDGE('',*,*,#7154,.T.);
#9577=ORIENTED_EDGE('',*,*,#7153,.F.);
#9578=ORIENTED_EDGE('',*,*,#7155,.F.);
#9579=ORIENTED_EDGE('',*,*,#7156,.T.);
#9580=ORIENTED_EDGE('',*,*,#7157,.T.);
#9581=ORIENTED_EDGE('',*,*,#7156,.F.);
#9582=ORIENTED_EDGE('',*,*,#7158,.F.);
#9583=ORIENTED_EDGE('',*,*,#7159,.T.);
#9584=ORIENTED_EDGE('',*,*,#7160,.T.);
#9585=ORIENTED_EDGE('',*,*,#7159,.F.);
#9586=ORIENTED_EDGE('',*,*,#7161,.F.);
#9587=ORIENTED_EDGE('',*,*,#7162,.T.);
#9588=ORIENTED_EDGE('',*,*,#7163,.T.);
#9589=ORIENTED_EDGE('',*,*,#7162,.F.);
#9590=ORIENTED_EDGE('',*,*,#7164,.F.);
#9591=ORIENTED_EDGE('',*,*,#7165,.T.);
#9592=ORIENTED_EDGE('',*,*,#7166,.T.);
#9593=ORIENTED_EDGE('',*,*,#7165,.F.);
#9594=ORIENTED_EDGE('',*,*,#7167,.F.);
#9595=ORIENTED_EDGE('',*,*,#7168,.T.);
#9596=ORIENTED_EDGE('',*,*,#7169,.T.);
#9597=ORIENTED_EDGE('',*,*,#7168,.F.);
#9598=ORIENTED_EDGE('',*,*,#7170,.F.);
#9599=ORIENTED_EDGE('',*,*,#7171,.T.);
#9600=ORIENTED_EDGE('',*,*,#7172,.T.);
#9601=ORIENTED_EDGE('',*,*,#7171,.F.);
#9602=ORIENTED_EDGE('',*,*,#7173,.F.);
#9603=ORIENTED_EDGE('',*,*,#7174,.T.);
#9604=ORIENTED_EDGE('',*,*,#7175,.T.);
#9605=ORIENTED_EDGE('',*,*,#7174,.F.);
#9606=ORIENTED_EDGE('',*,*,#7176,.F.);
#9607=ORIENTED_EDGE('',*,*,#7177,.T.);
#9608=ORIENTED_EDGE('',*,*,#7178,.T.);
#9609=ORIENTED_EDGE('',*,*,#7177,.F.);
#9610=ORIENTED_EDGE('',*,*,#7179,.F.);
#9611=ORIENTED_EDGE('',*,*,#7180,.T.);
#9612=ORIENTED_EDGE('',*,*,#7181,.T.);
#9613=ORIENTED_EDGE('',*,*,#7180,.F.);
#9614=ORIENTED_EDGE('',*,*,#7182,.F.);
#9615=ORIENTED_EDGE('',*,*,#7183,.T.);
#9616=ORIENTED_EDGE('',*,*,#7184,.T.);
#9617=ORIENTED_EDGE('',*,*,#7183,.F.);
#9618=ORIENTED_EDGE('',*,*,#7185,.F.);
#9619=ORIENTED_EDGE('',*,*,#7186,.T.);
#9620=ORIENTED_EDGE('',*,*,#7187,.T.);
#9621=ORIENTED_EDGE('',*,*,#7186,.F.);
#9622=ORIENTED_EDGE('',*,*,#7188,.F.);
#9623=ORIENTED_EDGE('',*,*,#7189,.T.);
#9624=ORIENTED_EDGE('',*,*,#7190,.T.);
#9625=ORIENTED_EDGE('',*,*,#7189,.F.);
#9626=ORIENTED_EDGE('',*,*,#7191,.F.);
#9627=ORIENTED_EDGE('',*,*,#7192,.T.);
#9628=ORIENTED_EDGE('',*,*,#7193,.T.);
#9629=ORIENTED_EDGE('',*,*,#7192,.F.);
#9630=ORIENTED_EDGE('',*,*,#7194,.F.);
#9631=ORIENTED_EDGE('',*,*,#7195,.T.);
#9632=ORIENTED_EDGE('',*,*,#7196,.T.);
#9633=ORIENTED_EDGE('',*,*,#7195,.F.);
#9634=ORIENTED_EDGE('',*,*,#7197,.F.);
#9635=ORIENTED_EDGE('',*,*,#7198,.T.);
#9636=ORIENTED_EDGE('',*,*,#7199,.T.);
#9637=ORIENTED_EDGE('',*,*,#7198,.F.);
#9638=ORIENTED_EDGE('',*,*,#7200,.F.);
#9639=ORIENTED_EDGE('',*,*,#7201,.T.);
#9640=ORIENTED_EDGE('',*,*,#7202,.T.);
#9641=ORIENTED_EDGE('',*,*,#7201,.F.);
#9642=ORIENTED_EDGE('',*,*,#7203,.F.);
#9643=ORIENTED_EDGE('',*,*,#7204,.T.);
#9644=ORIENTED_EDGE('',*,*,#7205,.T.);
#9645=ORIENTED_EDGE('',*,*,#7204,.F.);
#9646=ORIENTED_EDGE('',*,*,#7206,.F.);
#9647=ORIENTED_EDGE('',*,*,#7207,.T.);
#9648=ORIENTED_EDGE('',*,*,#7208,.T.);
#9649=ORIENTED_EDGE('',*,*,#7207,.F.);
#9650=ORIENTED_EDGE('',*,*,#7209,.F.);
#9651=ORIENTED_EDGE('',*,*,#7210,.T.);
#9652=ORIENTED_EDGE('',*,*,#7211,.T.);
#9653=ORIENTED_EDGE('',*,*,#7210,.F.);
#9654=ORIENTED_EDGE('',*,*,#7212,.F.);
#9655=ORIENTED_EDGE('',*,*,#6969,.T.);
#9656=ORIENTED_EDGE('',*,*,#7213,.F.);
#9657=ORIENTED_EDGE('',*,*,#7214,.F.);
#9658=ORIENTED_EDGE('',*,*,#6959,.F.);
#9659=ORIENTED_EDGE('',*,*,#6965,.F.);
#9660=ORIENTED_EDGE('',*,*,#6972,.F.);
#9661=ORIENTED_EDGE('',*,*,#7215,.F.);
#9662=ORIENTED_EDGE('',*,*,#7214,.T.);
#9663=ORIENTED_EDGE('',*,*,#7216,.F.);
#9664=ORIENTED_EDGE('',*,*,#6901,.F.);
#9665=ORIENTED_EDGE('',*,*,#6905,.T.);
#9666=ORIENTED_EDGE('',*,*,#6908,.F.);
#9667=ORIENTED_EDGE('',*,*,#6911,.F.);
#9668=ORIENTED_EDGE('',*,*,#7069,.T.);
#9669=ORIENTED_EDGE('',*,*,#7070,.F.);
#9670=ORIENTED_EDGE('',*,*,#6902,.F.);
#9671=ORIENTED_EDGE('',*,*,#7216,.T.);
#9672=ORIENTED_EDGE('',*,*,#7213,.T.);
#9673=ORIENTED_EDGE('',*,*,#6968,.T.);
#9674=ORIENTED_EDGE('',*,*,#7209,.T.);
#9675=ORIENTED_EDGE('',*,*,#7206,.T.);
#9676=ORIENTED_EDGE('',*,*,#7203,.T.);
#9677=ORIENTED_EDGE('',*,*,#7200,.T.);
#9678=ORIENTED_EDGE('',*,*,#7197,.T.);
#9679=ORIENTED_EDGE('',*,*,#7194,.T.);
#9680=ORIENTED_EDGE('',*,*,#7191,.T.);
#9681=ORIENTED_EDGE('',*,*,#7188,.T.);
#9682=ORIENTED_EDGE('',*,*,#7185,.T.);
#9683=ORIENTED_EDGE('',*,*,#7182,.T.);
#9684=ORIENTED_EDGE('',*,*,#7179,.T.);
#9685=ORIENTED_EDGE('',*,*,#7176,.T.);
#9686=ORIENTED_EDGE('',*,*,#7173,.T.);
#9687=ORIENTED_EDGE('',*,*,#7170,.T.);
#9688=ORIENTED_EDGE('',*,*,#7167,.T.);
#9689=ORIENTED_EDGE('',*,*,#7164,.T.);
#9690=ORIENTED_EDGE('',*,*,#7161,.T.);
#9691=ORIENTED_EDGE('',*,*,#7158,.T.);
#9692=ORIENTED_EDGE('',*,*,#7155,.T.);
#9693=ORIENTED_EDGE('',*,*,#7152,.T.);
#9694=ORIENTED_EDGE('',*,*,#7149,.T.);
#9695=ORIENTED_EDGE('',*,*,#7146,.T.);
#9696=ORIENTED_EDGE('',*,*,#7143,.T.);
#9697=ORIENTED_EDGE('',*,*,#7140,.T.);
#9698=ORIENTED_EDGE('',*,*,#7137,.T.);
#9699=ORIENTED_EDGE('',*,*,#7134,.T.);
#9700=ORIENTED_EDGE('',*,*,#7131,.T.);
#9701=ORIENTED_EDGE('',*,*,#7128,.T.);
#9702=ORIENTED_EDGE('',*,*,#7125,.T.);
#9703=ORIENTED_EDGE('',*,*,#7122,.T.);
#9704=ORIENTED_EDGE('',*,*,#7119,.T.);
#9705=ORIENTED_EDGE('',*,*,#7116,.T.);
#9706=ORIENTED_EDGE('',*,*,#7113,.T.);
#9707=ORIENTED_EDGE('',*,*,#7110,.T.);
#9708=ORIENTED_EDGE('',*,*,#7107,.T.);
#9709=ORIENTED_EDGE('',*,*,#7104,.T.);
#9710=ORIENTED_EDGE('',*,*,#7101,.T.);
#9711=ORIENTED_EDGE('',*,*,#7098,.T.);
#9712=ORIENTED_EDGE('',*,*,#7095,.T.);
#9713=ORIENTED_EDGE('',*,*,#7092,.T.);
#9714=ORIENTED_EDGE('',*,*,#7089,.T.);
#9715=ORIENTED_EDGE('',*,*,#7086,.T.);
#9716=ORIENTED_EDGE('',*,*,#7083,.T.);
#9717=ORIENTED_EDGE('',*,*,#7080,.T.);
#9718=ORIENTED_EDGE('',*,*,#7077,.T.);
#9719=ORIENTED_EDGE('',*,*,#7074,.T.);
#9720=ORIENTED_EDGE('',*,*,#7071,.T.);
#9721=ORIENTED_EDGE('',*,*,#6973,.F.);
#9722=ORIENTED_EDGE('',*,*,#6970,.T.);
#9723=ORIENTED_EDGE('',*,*,#7212,.T.);
#9724=ORIENTED_EDGE('',*,*,#7215,.T.);
#9725=ORIENTED_EDGE('',*,*,#7211,.F.);
#9726=ORIENTED_EDGE('',*,*,#7208,.F.);
#9727=ORIENTED_EDGE('',*,*,#7205,.F.);
#9728=ORIENTED_EDGE('',*,*,#7202,.F.);
#9729=ORIENTED_EDGE('',*,*,#7199,.F.);
#9730=ORIENTED_EDGE('',*,*,#7196,.F.);
#9731=ORIENTED_EDGE('',*,*,#7193,.F.);
#9732=ORIENTED_EDGE('',*,*,#7190,.F.);
#9733=ORIENTED_EDGE('',*,*,#7187,.F.);
#9734=ORIENTED_EDGE('',*,*,#7184,.F.);
#9735=ORIENTED_EDGE('',*,*,#7181,.F.);
#9736=ORIENTED_EDGE('',*,*,#7178,.F.);
#9737=ORIENTED_EDGE('',*,*,#7175,.F.);
#9738=ORIENTED_EDGE('',*,*,#7172,.F.);
#9739=ORIENTED_EDGE('',*,*,#7169,.F.);
#9740=ORIENTED_EDGE('',*,*,#7166,.F.);
#9741=ORIENTED_EDGE('',*,*,#7163,.F.);
#9742=ORIENTED_EDGE('',*,*,#7160,.F.);
#9743=ORIENTED_EDGE('',*,*,#7157,.F.);
#9744=ORIENTED_EDGE('',*,*,#7154,.F.);
#9745=ORIENTED_EDGE('',*,*,#7151,.F.);
#9746=ORIENTED_EDGE('',*,*,#7148,.F.);
#9747=ORIENTED_EDGE('',*,*,#7145,.F.);
#9748=ORIENTED_EDGE('',*,*,#7142,.F.);
#9749=ORIENTED_EDGE('',*,*,#7139,.F.);
#9750=ORIENTED_EDGE('',*,*,#7136,.F.);
#9751=ORIENTED_EDGE('',*,*,#7133,.F.);
#9752=ORIENTED_EDGE('',*,*,#7130,.F.);
#9753=ORIENTED_EDGE('',*,*,#7127,.F.);
#9754=ORIENTED_EDGE('',*,*,#7124,.F.);
#9755=ORIENTED_EDGE('',*,*,#7121,.F.);
#9756=ORIENTED_EDGE('',*,*,#7118,.F.);
#9757=ORIENTED_EDGE('',*,*,#7115,.F.);
#9758=ORIENTED_EDGE('',*,*,#7112,.F.);
#9759=ORIENTED_EDGE('',*,*,#7109,.F.);
#9760=ORIENTED_EDGE('',*,*,#7106,.F.);
#9761=ORIENTED_EDGE('',*,*,#7103,.F.);
#9762=ORIENTED_EDGE('',*,*,#7100,.F.);
#9763=ORIENTED_EDGE('',*,*,#7097,.F.);
#9764=ORIENTED_EDGE('',*,*,#7094,.F.);
#9765=ORIENTED_EDGE('',*,*,#7091,.F.);
#9766=ORIENTED_EDGE('',*,*,#7088,.F.);
#9767=ORIENTED_EDGE('',*,*,#7085,.F.);
#9768=ORIENTED_EDGE('',*,*,#7082,.F.);
#9769=ORIENTED_EDGE('',*,*,#7079,.F.);
#9770=ORIENTED_EDGE('',*,*,#7076,.F.);
#9771=ORIENTED_EDGE('',*,*,#7073,.F.);
#9772=ORIENTED_EDGE('',*,*,#7217,.F.);
#9773=ORIENTED_EDGE('',*,*,#7218,.T.);
#9774=ORIENTED_EDGE('',*,*,#7219,.F.);
#9775=ORIENTED_EDGE('',*,*,#7218,.F.);
#9776=ORIENTED_EDGE('',*,*,#7220,.F.);
#9777=ORIENTED_EDGE('',*,*,#7221,.T.);
#9778=ORIENTED_EDGE('',*,*,#7222,.F.);
#9779=ORIENTED_EDGE('',*,*,#7221,.F.);
#9780=ORIENTED_EDGE('',*,*,#7223,.F.);
#9781=ORIENTED_EDGE('',*,*,#7224,.T.);
#9782=ORIENTED_EDGE('',*,*,#7225,.F.);
#9783=ORIENTED_EDGE('',*,*,#7224,.F.);
#9784=ORIENTED_EDGE('',*,*,#7226,.T.);
#9785=ORIENTED_EDGE('',*,*,#7227,.T.);
#9786=ORIENTED_EDGE('',*,*,#7228,.T.);
#9787=ORIENTED_EDGE('',*,*,#7229,.T.);
#9788=ORIENTED_EDGE('',*,*,#7227,.F.);
#9789=ORIENTED_EDGE('',*,*,#7230,.T.);
#9790=ORIENTED_EDGE('',*,*,#7231,.F.);
#9791=ORIENTED_EDGE('',*,*,#7232,.T.);
#9792=ORIENTED_EDGE('',*,*,#7233,.T.);
#9793=ORIENTED_EDGE('',*,*,#7234,.F.);
#9794=ORIENTED_EDGE('',*,*,#7235,.T.);
#9795=ORIENTED_EDGE('',*,*,#7236,.T.);
#9796=ORIENTED_EDGE('',*,*,#7237,.F.);
#9797=ORIENTED_EDGE('',*,*,#7238,.F.);
#9798=ORIENTED_EDGE('',*,*,#7239,.F.);
#9799=ORIENTED_EDGE('',*,*,#7240,.F.);
#9800=ORIENTED_EDGE('',*,*,#7241,.F.);
#9801=ORIENTED_EDGE('',*,*,#7242,.F.);
#9802=ORIENTED_EDGE('',*,*,#7243,.F.);
#9803=ORIENTED_EDGE('',*,*,#7244,.F.);
#9804=ORIENTED_EDGE('',*,*,#7245,.F.);
#9805=ORIENTED_EDGE('',*,*,#7246,.F.);
#9806=ORIENTED_EDGE('',*,*,#7247,.F.);
#9807=ORIENTED_EDGE('',*,*,#7248,.T.);
#9808=ORIENTED_EDGE('',*,*,#7249,.T.);
#9809=ORIENTED_EDGE('',*,*,#7250,.T.);
#9810=ORIENTED_EDGE('',*,*,#7251,.F.);
#9811=ORIENTED_EDGE('',*,*,#7249,.F.);
#9812=ORIENTED_EDGE('',*,*,#7252,.T.);
#9813=ORIENTED_EDGE('',*,*,#7253,.T.);
#9814=ORIENTED_EDGE('',*,*,#7254,.T.);
#9815=ORIENTED_EDGE('',*,*,#7255,.T.);
#9816=ORIENTED_EDGE('',*,*,#7256,.T.);
#9817=ORIENTED_EDGE('',*,*,#7257,.T.);
#9818=ORIENTED_EDGE('',*,*,#7258,.T.);
#9819=ORIENTED_EDGE('',*,*,#7259,.T.);
#9820=ORIENTED_EDGE('',*,*,#7260,.T.);
#9821=ORIENTED_EDGE('',*,*,#7261,.T.);
#9822=ORIENTED_EDGE('',*,*,#7262,.T.);
#9823=ORIENTED_EDGE('',*,*,#7263,.T.);
#9824=ORIENTED_EDGE('',*,*,#7264,.T.);
#9825=ORIENTED_EDGE('',*,*,#7265,.T.);
#9826=ORIENTED_EDGE('',*,*,#7266,.T.);
#9827=ORIENTED_EDGE('',*,*,#7267,.T.);
#9828=ORIENTED_EDGE('',*,*,#7268,.T.);
#9829=ORIENTED_EDGE('',*,*,#7269,.T.);
#9830=ORIENTED_EDGE('',*,*,#7259,.F.);
#9831=ORIENTED_EDGE('',*,*,#7270,.T.);
#9832=ORIENTED_EDGE('',*,*,#7247,.T.);
#9833=ORIENTED_EDGE('',*,*,#7270,.F.);
#9834=ORIENTED_EDGE('',*,*,#7260,.F.);
#9835=ORIENTED_EDGE('',*,*,#7271,.T.);
#9836=ORIENTED_EDGE('',*,*,#7246,.T.);
#9837=ORIENTED_EDGE('',*,*,#7271,.F.);
#9838=ORIENTED_EDGE('',*,*,#7261,.F.);
#9839=ORIENTED_EDGE('',*,*,#7272,.T.);
#9840=ORIENTED_EDGE('',*,*,#7245,.T.);
#9841=ORIENTED_EDGE('',*,*,#7272,.F.);
#9842=ORIENTED_EDGE('',*,*,#7262,.F.);
#9843=ORIENTED_EDGE('',*,*,#7273,.T.);
#9844=ORIENTED_EDGE('',*,*,#7244,.T.);
#9845=ORIENTED_EDGE('',*,*,#7273,.F.);
#9846=ORIENTED_EDGE('',*,*,#7263,.F.);
#9847=ORIENTED_EDGE('',*,*,#7274,.T.);
#9848=ORIENTED_EDGE('',*,*,#7243,.T.);
#9849=ORIENTED_EDGE('',*,*,#7274,.F.);
#9850=ORIENTED_EDGE('',*,*,#7264,.F.);
#9851=ORIENTED_EDGE('',*,*,#7275,.T.);
#9852=ORIENTED_EDGE('',*,*,#7242,.T.);
#9853=ORIENTED_EDGE('',*,*,#7275,.F.);
#9854=ORIENTED_EDGE('',*,*,#7265,.F.);
#9855=ORIENTED_EDGE('',*,*,#7276,.T.);
#9856=ORIENTED_EDGE('',*,*,#7241,.T.);
#9857=ORIENTED_EDGE('',*,*,#7276,.F.);
#9858=ORIENTED_EDGE('',*,*,#7266,.F.);
#9859=ORIENTED_EDGE('',*,*,#7277,.T.);
#9860=ORIENTED_EDGE('',*,*,#7240,.T.);
#9861=ORIENTED_EDGE('',*,*,#7277,.F.);
#9862=ORIENTED_EDGE('',*,*,#7267,.F.);
#9863=ORIENTED_EDGE('',*,*,#7278,.T.);
#9864=ORIENTED_EDGE('',*,*,#7239,.T.);
#9865=ORIENTED_EDGE('',*,*,#7278,.F.);
#9866=ORIENTED_EDGE('',*,*,#7268,.F.);
#9867=ORIENTED_EDGE('',*,*,#7279,.T.);
#9868=ORIENTED_EDGE('',*,*,#7238,.T.);
#9869=ORIENTED_EDGE('',*,*,#7279,.F.);
#9870=ORIENTED_EDGE('',*,*,#7269,.F.);
#9871=ORIENTED_EDGE('',*,*,#7280,.T.);
#9872=ORIENTED_EDGE('',*,*,#7237,.T.);
#9873=ORIENTED_EDGE('',*,*,#7280,.F.);
#9874=ORIENTED_EDGE('',*,*,#7235,.F.);
#9875=ORIENTED_EDGE('',*,*,#7281,.T.);
#9876=ORIENTED_EDGE('',*,*,#7253,.F.);
#9877=ORIENTED_EDGE('',*,*,#7282,.F.);
#9878=ORIENTED_EDGE('',*,*,#7231,.T.);
#9879=ORIENTED_EDGE('',*,*,#7283,.T.);
#9880=ORIENTED_EDGE('',*,*,#7257,.F.);
#9881=ORIENTED_EDGE('',*,*,#7284,.F.);
#9882=ORIENTED_EDGE('',*,*,#7232,.F.);
#9883=ORIENTED_EDGE('',*,*,#7284,.T.);
#9884=ORIENTED_EDGE('',*,*,#7256,.F.);
#9885=ORIENTED_EDGE('',*,*,#7285,.F.);
#9886=ORIENTED_EDGE('',*,*,#7233,.F.);
#9887=ORIENTED_EDGE('',*,*,#7285,.T.);
#9888=ORIENTED_EDGE('',*,*,#7255,.F.);
#9889=ORIENTED_EDGE('',*,*,#7286,.F.);
#9890=ORIENTED_EDGE('',*,*,#7234,.T.);
#9891=ORIENTED_EDGE('',*,*,#7286,.T.);
#9892=ORIENTED_EDGE('',*,*,#7254,.F.);
#9893=ORIENTED_EDGE('',*,*,#7281,.F.);
#9894=ORIENTED_EDGE('',*,*,#7287,.F.);
#9895=ORIENTED_EDGE('',*,*,#7288,.T.);
#9896=ORIENTED_EDGE('',*,*,#7289,.F.);
#9897=ORIENTED_EDGE('',*,*,#7290,.T.);
#9898=ORIENTED_EDGE('',*,*,#7291,.T.);
#9899=ORIENTED_EDGE('',*,*,#7292,.F.);
#9900=ORIENTED_EDGE('',*,*,#7293,.T.);
#9901=ORIENTED_EDGE('',*,*,#7294,.T.);
#9902=ORIENTED_EDGE('',*,*,#7295,.F.);
#9903=ORIENTED_EDGE('',*,*,#7296,.F.);
#9904=ORIENTED_EDGE('',*,*,#7297,.F.);
#9905=ORIENTED_EDGE('',*,*,#7298,.F.);
#9906=ORIENTED_EDGE('',*,*,#7299,.F.);
#9907=ORIENTED_EDGE('',*,*,#7300,.F.);
#9908=ORIENTED_EDGE('',*,*,#7301,.F.);
#9909=ORIENTED_EDGE('',*,*,#7302,.F.);
#9910=ORIENTED_EDGE('',*,*,#7303,.F.);
#9911=ORIENTED_EDGE('',*,*,#7304,.F.);
#9912=ORIENTED_EDGE('',*,*,#7305,.F.);
#9913=ORIENTED_EDGE('',*,*,#7306,.F.);
#9914=ORIENTED_EDGE('',*,*,#7307,.T.);
#9915=ORIENTED_EDGE('',*,*,#7295,.T.);
#9916=ORIENTED_EDGE('',*,*,#7307,.F.);
#9917=ORIENTED_EDGE('',*,*,#7308,.F.);
#9918=ORIENTED_EDGE('',*,*,#7309,.T.);
#9919=ORIENTED_EDGE('',*,*,#7296,.T.);
#9920=ORIENTED_EDGE('',*,*,#7309,.F.);
#9921=ORIENTED_EDGE('',*,*,#7310,.F.);
#9922=ORIENTED_EDGE('',*,*,#7311,.T.);
#9923=ORIENTED_EDGE('',*,*,#7297,.T.);
#9924=ORIENTED_EDGE('',*,*,#7311,.F.);
#9925=ORIENTED_EDGE('',*,*,#7312,.F.);
#9926=ORIENTED_EDGE('',*,*,#7313,.T.);
#9927=ORIENTED_EDGE('',*,*,#7298,.T.);
#9928=ORIENTED_EDGE('',*,*,#7313,.F.);
#9929=ORIENTED_EDGE('',*,*,#7314,.F.);
#9930=ORIENTED_EDGE('',*,*,#7315,.T.);
#9931=ORIENTED_EDGE('',*,*,#7299,.T.);
#9932=ORIENTED_EDGE('',*,*,#7315,.F.);
#9933=ORIENTED_EDGE('',*,*,#7316,.F.);
#9934=ORIENTED_EDGE('',*,*,#7317,.T.);
#9935=ORIENTED_EDGE('',*,*,#7300,.T.);
#9936=ORIENTED_EDGE('',*,*,#7317,.F.);
#9937=ORIENTED_EDGE('',*,*,#7318,.F.);
#9938=ORIENTED_EDGE('',*,*,#7319,.T.);
#9939=ORIENTED_EDGE('',*,*,#7301,.T.);
#9940=ORIENTED_EDGE('',*,*,#7319,.F.);
#9941=ORIENTED_EDGE('',*,*,#7320,.F.);
#9942=ORIENTED_EDGE('',*,*,#7321,.T.);
#9943=ORIENTED_EDGE('',*,*,#7302,.T.);
#9944=ORIENTED_EDGE('',*,*,#7321,.F.);
#9945=ORIENTED_EDGE('',*,*,#7322,.F.);
#9946=ORIENTED_EDGE('',*,*,#7323,.T.);
#9947=ORIENTED_EDGE('',*,*,#7303,.T.);
#9948=ORIENTED_EDGE('',*,*,#7323,.F.);
#9949=ORIENTED_EDGE('',*,*,#7324,.F.);
#9950=ORIENTED_EDGE('',*,*,#7325,.T.);
#9951=ORIENTED_EDGE('',*,*,#7304,.T.);
#9952=ORIENTED_EDGE('',*,*,#7325,.F.);
#9953=ORIENTED_EDGE('',*,*,#7326,.F.);
#9954=ORIENTED_EDGE('',*,*,#7327,.T.);
#9955=ORIENTED_EDGE('',*,*,#7305,.T.);
#9956=ORIENTED_EDGE('',*,*,#7327,.F.);
#9957=ORIENTED_EDGE('',*,*,#7293,.F.);
#9958=ORIENTED_EDGE('',*,*,#7328,.T.);
#9959=ORIENTED_EDGE('',*,*,#7329,.F.);
#9960=ORIENTED_EDGE('',*,*,#7330,.F.);
#9961=ORIENTED_EDGE('',*,*,#7289,.T.);
#9962=ORIENTED_EDGE('',*,*,#7331,.T.);
#9963=ORIENTED_EDGE('',*,*,#7332,.F.);
#9964=ORIENTED_EDGE('',*,*,#7333,.F.);
#9965=ORIENTED_EDGE('',*,*,#7290,.F.);
#9966=ORIENTED_EDGE('',*,*,#7333,.T.);
#9967=ORIENTED_EDGE('',*,*,#7334,.F.);
#9968=ORIENTED_EDGE('',*,*,#7335,.F.);
#9969=ORIENTED_EDGE('',*,*,#7291,.F.);
#9970=ORIENTED_EDGE('',*,*,#7335,.T.);
#9971=ORIENTED_EDGE('',*,*,#7336,.F.);
#9972=ORIENTED_EDGE('',*,*,#7337,.F.);
#9973=ORIENTED_EDGE('',*,*,#7292,.T.);
#9974=ORIENTED_EDGE('',*,*,#7337,.T.);
#9975=ORIENTED_EDGE('',*,*,#7338,.F.);
#9976=ORIENTED_EDGE('',*,*,#7328,.F.);
#9977=ORIENTED_EDGE('',*,*,#7339,.F.);
#9978=ORIENTED_EDGE('',*,*,#7340,.T.);
#9979=ORIENTED_EDGE('',*,*,#7329,.T.);
#9980=ORIENTED_EDGE('',*,*,#7338,.T.);
#9981=ORIENTED_EDGE('',*,*,#7336,.T.);
#9982=ORIENTED_EDGE('',*,*,#7334,.T.);
#9983=ORIENTED_EDGE('',*,*,#7332,.T.);
#9984=ORIENTED_EDGE('',*,*,#7341,.T.);
#9985=ORIENTED_EDGE('',*,*,#7306,.T.);
#9986=ORIENTED_EDGE('',*,*,#7308,.T.);
#9987=ORIENTED_EDGE('',*,*,#7310,.T.);
#9988=ORIENTED_EDGE('',*,*,#7312,.T.);
#9989=ORIENTED_EDGE('',*,*,#7314,.T.);
#9990=ORIENTED_EDGE('',*,*,#7316,.T.);
#9991=ORIENTED_EDGE('',*,*,#7318,.T.);
#9992=ORIENTED_EDGE('',*,*,#7320,.T.);
#9993=ORIENTED_EDGE('',*,*,#7322,.T.);
#9994=ORIENTED_EDGE('',*,*,#7324,.T.);
#9995=ORIENTED_EDGE('',*,*,#7326,.T.);
#9996=ORIENTED_EDGE('',*,*,#7342,.F.);
#9997=ORIENTED_EDGE('',*,*,#7251,.T.);
#9998=ORIENTED_EDGE('',*,*,#7343,.T.);
#9999=ORIENTED_EDGE('',*,*,#7344,.F.);
#10000=ORIENTED_EDGE('',*,*,#7219,.T.);
#10001=ORIENTED_EDGE('',*,*,#7220,.T.);
#10002=ORIENTED_EDGE('',*,*,#7223,.T.);
#10003=ORIENTED_EDGE('',*,*,#7229,.F.);
#10004=ORIENTED_EDGE('',*,*,#7345,.T.);
#10005=ORIENTED_EDGE('',*,*,#7339,.T.);
#10006=ORIENTED_EDGE('',*,*,#7346,.F.);
#10007=ORIENTED_EDGE('',*,*,#7217,.T.);
#10008=ORIENTED_EDGE('',*,*,#7342,.T.);
#10009=ORIENTED_EDGE('',*,*,#7347,.F.);
#10010=ORIENTED_EDGE('',*,*,#7348,.F.);
#10011=ORIENTED_EDGE('',*,*,#7294,.F.);
#10012=ORIENTED_EDGE('',*,*,#7330,.T.);
#10013=ORIENTED_EDGE('',*,*,#7340,.F.);
#10014=ORIENTED_EDGE('',*,*,#7345,.F.);
#10015=ORIENTED_EDGE('',*,*,#7228,.F.);
#10016=ORIENTED_EDGE('',*,*,#7236,.F.);
#10017=ORIENTED_EDGE('',*,*,#7282,.T.);
#10018=ORIENTED_EDGE('',*,*,#7252,.F.);
#10019=ORIENTED_EDGE('',*,*,#7248,.F.);
#10020=ORIENTED_EDGE('',*,*,#7287,.T.);
#10021=ORIENTED_EDGE('',*,*,#7348,.T.);
#10022=ORIENTED_EDGE('',*,*,#7349,.F.);
#10023=ORIENTED_EDGE('',*,*,#7350,.F.);
#10024=ORIENTED_EDGE('',*,*,#7222,.T.);
#10025=ORIENTED_EDGE('',*,*,#7225,.T.);
#10026=ORIENTED_EDGE('',*,*,#7343,.F.);
#10027=ORIENTED_EDGE('',*,*,#7250,.F.);
#10028=ORIENTED_EDGE('',*,*,#7258,.F.);
#10029=ORIENTED_EDGE('',*,*,#7283,.F.);
#10030=ORIENTED_EDGE('',*,*,#7230,.F.);
#10031=ORIENTED_EDGE('',*,*,#7226,.F.);
#10032=ORIENTED_EDGE('',*,*,#7346,.T.);
#10033=ORIENTED_EDGE('',*,*,#7341,.F.);
#10034=ORIENTED_EDGE('',*,*,#7331,.F.);
#10035=ORIENTED_EDGE('',*,*,#7288,.F.);
#10036=ORIENTED_EDGE('',*,*,#7350,.T.);
#10037=ORIENTED_EDGE('',*,*,#7351,.F.);
#10038=ORIENTED_EDGE('',*,*,#7344,.T.);
#10039=ORIENTED_EDGE('',*,*,#7351,.T.);
#10040=ORIENTED_EDGE('',*,*,#7349,.T.);
#10041=ORIENTED_EDGE('',*,*,#7347,.T.);
#10042=ORIENTED_EDGE('',*,*,#7352,.F.);
#10043=ORIENTED_EDGE('',*,*,#7353,.T.);
#10044=ORIENTED_EDGE('',*,*,#7354,.F.);
#10045=ORIENTED_EDGE('',*,*,#7353,.F.);
#10046=ORIENTED_EDGE('',*,*,#7355,.F.);
#10047=ORIENTED_EDGE('',*,*,#7356,.T.);
#10048=ORIENTED_EDGE('',*,*,#7357,.F.);
#10049=ORIENTED_EDGE('',*,*,#7358,.F.);
#10050=ORIENTED_EDGE('',*,*,#7359,.F.);
#10051=ORIENTED_EDGE('',*,*,#7358,.T.);
#10052=ORIENTED_EDGE('',*,*,#7360,.F.);
#10053=ORIENTED_EDGE('',*,*,#7361,.F.);
#10054=ORIENTED_EDGE('',*,*,#7362,.F.);
#10055=ORIENTED_EDGE('',*,*,#7361,.T.);
#10056=ORIENTED_EDGE('',*,*,#7363,.F.);
#10057=ORIENTED_EDGE('',*,*,#7364,.F.);
#10058=ORIENTED_EDGE('',*,*,#7365,.F.);
#10059=ORIENTED_EDGE('',*,*,#7364,.T.);
#10060=ORIENTED_EDGE('',*,*,#7366,.F.);
#10061=ORIENTED_EDGE('',*,*,#7367,.F.);
#10062=ORIENTED_EDGE('',*,*,#7368,.F.);
#10063=ORIENTED_EDGE('',*,*,#7367,.T.);
#10064=ORIENTED_EDGE('',*,*,#7369,.F.);
#10065=ORIENTED_EDGE('',*,*,#7370,.F.);
#10066=ORIENTED_EDGE('',*,*,#7371,.F.);
#10067=ORIENTED_EDGE('',*,*,#7370,.T.);
#10068=ORIENTED_EDGE('',*,*,#7372,.F.);
#10069=ORIENTED_EDGE('',*,*,#7356,.F.);
#10070=ORIENTED_EDGE('',*,*,#7371,.T.);
#10071=ORIENTED_EDGE('',*,*,#7355,.T.);
#10072=ORIENTED_EDGE('',*,*,#7359,.T.);
#10073=ORIENTED_EDGE('',*,*,#7362,.T.);
#10074=ORIENTED_EDGE('',*,*,#7365,.T.);
#10075=ORIENTED_EDGE('',*,*,#7368,.T.);
#10076=ORIENTED_EDGE('',*,*,#7354,.T.);
#10077=ORIENTED_EDGE('',*,*,#7372,.T.);
#10078=ORIENTED_EDGE('',*,*,#7369,.T.);
#10079=ORIENTED_EDGE('',*,*,#7366,.T.);
#10080=ORIENTED_EDGE('',*,*,#7363,.T.);
#10081=ORIENTED_EDGE('',*,*,#7360,.T.);
#10082=ORIENTED_EDGE('',*,*,#7357,.T.);
#10083=ORIENTED_EDGE('',*,*,#7352,.T.);
#10084=ORIENTED_EDGE('',*,*,#7373,.F.);
#10085=ORIENTED_EDGE('',*,*,#7374,.T.);
#10086=ORIENTED_EDGE('',*,*,#7375,.F.);
#10087=ORIENTED_EDGE('',*,*,#7374,.F.);
#10088=ORIENTED_EDGE('',*,*,#7376,.F.);
#10089=ORIENTED_EDGE('',*,*,#7377,.T.);
#10090=ORIENTED_EDGE('',*,*,#7378,.F.);
#10091=ORIENTED_EDGE('',*,*,#7377,.F.);
#10092=ORIENTED_EDGE('',*,*,#7379,.F.);
#10093=ORIENTED_EDGE('',*,*,#7380,.T.);
#10094=ORIENTED_EDGE('',*,*,#7381,.F.);
#10095=ORIENTED_EDGE('',*,*,#7380,.F.);
#10096=ORIENTED_EDGE('',*,*,#7382,.T.);
#10097=ORIENTED_EDGE('',*,*,#7383,.T.);
#10098=ORIENTED_EDGE('',*,*,#7384,.T.);
#10099=ORIENTED_EDGE('',*,*,#7385,.T.);
#10100=ORIENTED_EDGE('',*,*,#7383,.F.);
#10101=ORIENTED_EDGE('',*,*,#7386,.T.);
#10102=ORIENTED_EDGE('',*,*,#7387,.F.);
#10103=ORIENTED_EDGE('',*,*,#7388,.T.);
#10104=ORIENTED_EDGE('',*,*,#7389,.T.);
#10105=ORIENTED_EDGE('',*,*,#7390,.F.);
#10106=ORIENTED_EDGE('',*,*,#7391,.T.);
#10107=ORIENTED_EDGE('',*,*,#7392,.T.);
#10108=ORIENTED_EDGE('',*,*,#7393,.F.);
#10109=ORIENTED_EDGE('',*,*,#7394,.F.);
#10110=ORIENTED_EDGE('',*,*,#7395,.F.);
#10111=ORIENTED_EDGE('',*,*,#7396,.F.);
#10112=ORIENTED_EDGE('',*,*,#7397,.F.);
#10113=ORIENTED_EDGE('',*,*,#7398,.F.);
#10114=ORIENTED_EDGE('',*,*,#7399,.F.);
#10115=ORIENTED_EDGE('',*,*,#7400,.F.);
#10116=ORIENTED_EDGE('',*,*,#7401,.F.);
#10117=ORIENTED_EDGE('',*,*,#7402,.F.);
#10118=ORIENTED_EDGE('',*,*,#7403,.F.);
#10119=ORIENTED_EDGE('',*,*,#7404,.T.);
#10120=ORIENTED_EDGE('',*,*,#7405,.T.);
#10121=ORIENTED_EDGE('',*,*,#7406,.T.);
#10122=ORIENTED_EDGE('',*,*,#7407,.F.);
#10123=ORIENTED_EDGE('',*,*,#7405,.F.);
#10124=ORIENTED_EDGE('',*,*,#7408,.T.);
#10125=ORIENTED_EDGE('',*,*,#7409,.T.);
#10126=ORIENTED_EDGE('',*,*,#7410,.T.);
#10127=ORIENTED_EDGE('',*,*,#7411,.T.);
#10128=ORIENTED_EDGE('',*,*,#7412,.T.);
#10129=ORIENTED_EDGE('',*,*,#7413,.T.);
#10130=ORIENTED_EDGE('',*,*,#7414,.T.);
#10131=ORIENTED_EDGE('',*,*,#7415,.T.);
#10132=ORIENTED_EDGE('',*,*,#7416,.T.);
#10133=ORIENTED_EDGE('',*,*,#7417,.T.);
#10134=ORIENTED_EDGE('',*,*,#7418,.T.);
#10135=ORIENTED_EDGE('',*,*,#7419,.T.);
#10136=ORIENTED_EDGE('',*,*,#7420,.T.);
#10137=ORIENTED_EDGE('',*,*,#7421,.T.);
#10138=ORIENTED_EDGE('',*,*,#7422,.T.);
#10139=ORIENTED_EDGE('',*,*,#7423,.T.);
#10140=ORIENTED_EDGE('',*,*,#7424,.T.);
#10141=ORIENTED_EDGE('',*,*,#7425,.T.);
#10142=ORIENTED_EDGE('',*,*,#7415,.F.);
#10143=ORIENTED_EDGE('',*,*,#7426,.T.);
#10144=ORIENTED_EDGE('',*,*,#7403,.T.);
#10145=ORIENTED_EDGE('',*,*,#7426,.F.);
#10146=ORIENTED_EDGE('',*,*,#7416,.F.);
#10147=ORIENTED_EDGE('',*,*,#7427,.T.);
#10148=ORIENTED_EDGE('',*,*,#7402,.T.);
#10149=ORIENTED_EDGE('',*,*,#7427,.F.);
#10150=ORIENTED_EDGE('',*,*,#7417,.F.);
#10151=ORIENTED_EDGE('',*,*,#7428,.T.);
#10152=ORIENTED_EDGE('',*,*,#7401,.T.);
#10153=ORIENTED_EDGE('',*,*,#7428,.F.);
#10154=ORIENTED_EDGE('',*,*,#7418,.F.);
#10155=ORIENTED_EDGE('',*,*,#7429,.T.);
#10156=ORIENTED_EDGE('',*,*,#7400,.T.);
#10157=ORIENTED_EDGE('',*,*,#7429,.F.);
#10158=ORIENTED_EDGE('',*,*,#7419,.F.);
#10159=ORIENTED_EDGE('',*,*,#7430,.T.);
#10160=ORIENTED_EDGE('',*,*,#7399,.T.);
#10161=ORIENTED_EDGE('',*,*,#7430,.F.);
#10162=ORIENTED_EDGE('',*,*,#7420,.F.);
#10163=ORIENTED_EDGE('',*,*,#7431,.T.);
#10164=ORIENTED_EDGE('',*,*,#7398,.T.);
#10165=ORIENTED_EDGE('',*,*,#7431,.F.);
#10166=ORIENTED_EDGE('',*,*,#7421,.F.);
#10167=ORIENTED_EDGE('',*,*,#7432,.T.);
#10168=ORIENTED_EDGE('',*,*,#7397,.T.);
#10169=ORIENTED_EDGE('',*,*,#7432,.F.);
#10170=ORIENTED_EDGE('',*,*,#7422,.F.);
#10171=ORIENTED_EDGE('',*,*,#7433,.T.);
#10172=ORIENTED_EDGE('',*,*,#7396,.T.);
#10173=ORIENTED_EDGE('',*,*,#7433,.F.);
#10174=ORIENTED_EDGE('',*,*,#7423,.F.);
#10175=ORIENTED_EDGE('',*,*,#7434,.T.);
#10176=ORIENTED_EDGE('',*,*,#7395,.T.);
#10177=ORIENTED_EDGE('',*,*,#7434,.F.);
#10178=ORIENTED_EDGE('',*,*,#7424,.F.);
#10179=ORIENTED_EDGE('',*,*,#7435,.T.);
#10180=ORIENTED_EDGE('',*,*,#7394,.T.);
#10181=ORIENTED_EDGE('',*,*,#7435,.F.);
#10182=ORIENTED_EDGE('',*,*,#7425,.F.);
#10183=ORIENTED_EDGE('',*,*,#7436,.T.);
#10184=ORIENTED_EDGE('',*,*,#7393,.T.);
#10185=ORIENTED_EDGE('',*,*,#7436,.F.);
#10186=ORIENTED_EDGE('',*,*,#7391,.F.);
#10187=ORIENTED_EDGE('',*,*,#7437,.T.);
#10188=ORIENTED_EDGE('',*,*,#7409,.F.);
#10189=ORIENTED_EDGE('',*,*,#7438,.F.);
#10190=ORIENTED_EDGE('',*,*,#7387,.T.);
#10191=ORIENTED_EDGE('',*,*,#7439,.T.);
#10192=ORIENTED_EDGE('',*,*,#7413,.F.);
#10193=ORIENTED_EDGE('',*,*,#7440,.F.);
#10194=ORIENTED_EDGE('',*,*,#7388,.F.);
#10195=ORIENTED_EDGE('',*,*,#7440,.T.);
#10196=ORIENTED_EDGE('',*,*,#7412,.F.);
#10197=ORIENTED_EDGE('',*,*,#7441,.F.);
#10198=ORIENTED_EDGE('',*,*,#7389,.F.);
#10199=ORIENTED_EDGE('',*,*,#7441,.T.);
#10200=ORIENTED_EDGE('',*,*,#7411,.F.);
#10201=ORIENTED_EDGE('',*,*,#7442,.F.);
#10202=ORIENTED_EDGE('',*,*,#7390,.T.);
#10203=ORIENTED_EDGE('',*,*,#7442,.T.);
#10204=ORIENTED_EDGE('',*,*,#7410,.F.);
#10205=ORIENTED_EDGE('',*,*,#7437,.F.);
#10206=ORIENTED_EDGE('',*,*,#7443,.F.);
#10207=ORIENTED_EDGE('',*,*,#7444,.T.);
#10208=ORIENTED_EDGE('',*,*,#7445,.F.);
#10209=ORIENTED_EDGE('',*,*,#7446,.T.);
#10210=ORIENTED_EDGE('',*,*,#7447,.T.);
#10211=ORIENTED_EDGE('',*,*,#7448,.F.);
#10212=ORIENTED_EDGE('',*,*,#7449,.T.);
#10213=ORIENTED_EDGE('',*,*,#7450,.T.);
#10214=ORIENTED_EDGE('',*,*,#7451,.F.);
#10215=ORIENTED_EDGE('',*,*,#7452,.F.);
#10216=ORIENTED_EDGE('',*,*,#7453,.F.);
#10217=ORIENTED_EDGE('',*,*,#7454,.F.);
#10218=ORIENTED_EDGE('',*,*,#7455,.F.);
#10219=ORIENTED_EDGE('',*,*,#7456,.F.);
#10220=ORIENTED_EDGE('',*,*,#7457,.F.);
#10221=ORIENTED_EDGE('',*,*,#7458,.F.);
#10222=ORIENTED_EDGE('',*,*,#7459,.F.);
#10223=ORIENTED_EDGE('',*,*,#7460,.F.);
#10224=ORIENTED_EDGE('',*,*,#7461,.F.);
#10225=ORIENTED_EDGE('',*,*,#7462,.F.);
#10226=ORIENTED_EDGE('',*,*,#7463,.T.);
#10227=ORIENTED_EDGE('',*,*,#7451,.T.);
#10228=ORIENTED_EDGE('',*,*,#7463,.F.);
#10229=ORIENTED_EDGE('',*,*,#7464,.F.);
#10230=ORIENTED_EDGE('',*,*,#7465,.T.);
#10231=ORIENTED_EDGE('',*,*,#7452,.T.);
#10232=ORIENTED_EDGE('',*,*,#7465,.F.);
#10233=ORIENTED_EDGE('',*,*,#7466,.F.);
#10234=ORIENTED_EDGE('',*,*,#7467,.T.);
#10235=ORIENTED_EDGE('',*,*,#7453,.T.);
#10236=ORIENTED_EDGE('',*,*,#7467,.F.);
#10237=ORIENTED_EDGE('',*,*,#7468,.F.);
#10238=ORIENTED_EDGE('',*,*,#7469,.T.);
#10239=ORIENTED_EDGE('',*,*,#7454,.T.);
#10240=ORIENTED_EDGE('',*,*,#7469,.F.);
#10241=ORIENTED_EDGE('',*,*,#7470,.F.);
#10242=ORIENTED_EDGE('',*,*,#7471,.T.);
#10243=ORIENTED_EDGE('',*,*,#7455,.T.);
#10244=ORIENTED_EDGE('',*,*,#7471,.F.);
#10245=ORIENTED_EDGE('',*,*,#7472,.F.);
#10246=ORIENTED_EDGE('',*,*,#7473,.T.);
#10247=ORIENTED_EDGE('',*,*,#7456,.T.);
#10248=ORIENTED_EDGE('',*,*,#7473,.F.);
#10249=ORIENTED_EDGE('',*,*,#7474,.F.);
#10250=ORIENTED_EDGE('',*,*,#7475,.T.);
#10251=ORIENTED_EDGE('',*,*,#7457,.T.);
#10252=ORIENTED_EDGE('',*,*,#7475,.F.);
#10253=ORIENTED_EDGE('',*,*,#7476,.F.);
#10254=ORIENTED_EDGE('',*,*,#7477,.T.);
#10255=ORIENTED_EDGE('',*,*,#7458,.T.);
#10256=ORIENTED_EDGE('',*,*,#7477,.F.);
#10257=ORIENTED_EDGE('',*,*,#7478,.F.);
#10258=ORIENTED_EDGE('',*,*,#7479,.T.);
#10259=ORIENTED_EDGE('',*,*,#7459,.T.);
#10260=ORIENTED_EDGE('',*,*,#7479,.F.);
#10261=ORIENTED_EDGE('',*,*,#7480,.F.);
#10262=ORIENTED_EDGE('',*,*,#7481,.T.);
#10263=ORIENTED_EDGE('',*,*,#7460,.T.);
#10264=ORIENTED_EDGE('',*,*,#7481,.F.);
#10265=ORIENTED_EDGE('',*,*,#7482,.F.);
#10266=ORIENTED_EDGE('',*,*,#7483,.T.);
#10267=ORIENTED_EDGE('',*,*,#7461,.T.);
#10268=ORIENTED_EDGE('',*,*,#7483,.F.);
#10269=ORIENTED_EDGE('',*,*,#7449,.F.);
#10270=ORIENTED_EDGE('',*,*,#7484,.T.);
#10271=ORIENTED_EDGE('',*,*,#7485,.F.);
#10272=ORIENTED_EDGE('',*,*,#7486,.F.);
#10273=ORIENTED_EDGE('',*,*,#7445,.T.);
#10274=ORIENTED_EDGE('',*,*,#7487,.T.);
#10275=ORIENTED_EDGE('',*,*,#7488,.F.);
#10276=ORIENTED_EDGE('',*,*,#7489,.F.);
#10277=ORIENTED_EDGE('',*,*,#7446,.F.);
#10278=ORIENTED_EDGE('',*,*,#7489,.T.);
#10279=ORIENTED_EDGE('',*,*,#7490,.F.);
#10280=ORIENTED_EDGE('',*,*,#7491,.F.);
#10281=ORIENTED_EDGE('',*,*,#7447,.F.);
#10282=ORIENTED_EDGE('',*,*,#7491,.T.);
#10283=ORIENTED_EDGE('',*,*,#7492,.F.);
#10284=ORIENTED_EDGE('',*,*,#7493,.F.);
#10285=ORIENTED_EDGE('',*,*,#7448,.T.);
#10286=ORIENTED_EDGE('',*,*,#7493,.T.);
#10287=ORIENTED_EDGE('',*,*,#7494,.F.);
#10288=ORIENTED_EDGE('',*,*,#7484,.F.);
#10289=ORIENTED_EDGE('',*,*,#7495,.F.);
#10290=ORIENTED_EDGE('',*,*,#7496,.T.);
#10291=ORIENTED_EDGE('',*,*,#7485,.T.);
#10292=ORIENTED_EDGE('',*,*,#7494,.T.);
#10293=ORIENTED_EDGE('',*,*,#7492,.T.);
#10294=ORIENTED_EDGE('',*,*,#7490,.T.);
#10295=ORIENTED_EDGE('',*,*,#7488,.T.);
#10296=ORIENTED_EDGE('',*,*,#7497,.T.);
#10297=ORIENTED_EDGE('',*,*,#7462,.T.);
#10298=ORIENTED_EDGE('',*,*,#7464,.T.);
#10299=ORIENTED_EDGE('',*,*,#7466,.T.);
#10300=ORIENTED_EDGE('',*,*,#7468,.T.);
#10301=ORIENTED_EDGE('',*,*,#7470,.T.);
#10302=ORIENTED_EDGE('',*,*,#7472,.T.);
#10303=ORIENTED_EDGE('',*,*,#7474,.T.);
#10304=ORIENTED_EDGE('',*,*,#7476,.T.);
#10305=ORIENTED_EDGE('',*,*,#7478,.T.);
#10306=ORIENTED_EDGE('',*,*,#7480,.T.);
#10307=ORIENTED_EDGE('',*,*,#7482,.T.);
#10308=ORIENTED_EDGE('',*,*,#7498,.F.);
#10309=ORIENTED_EDGE('',*,*,#7407,.T.);
#10310=ORIENTED_EDGE('',*,*,#7499,.T.);
#10311=ORIENTED_EDGE('',*,*,#7500,.F.);
#10312=ORIENTED_EDGE('',*,*,#7375,.T.);
#10313=ORIENTED_EDGE('',*,*,#7376,.T.);
#10314=ORIENTED_EDGE('',*,*,#7379,.T.);
#10315=ORIENTED_EDGE('',*,*,#7385,.F.);
#10316=ORIENTED_EDGE('',*,*,#7501,.T.);
#10317=ORIENTED_EDGE('',*,*,#7495,.T.);
#10318=ORIENTED_EDGE('',*,*,#7502,.F.);
#10319=ORIENTED_EDGE('',*,*,#7373,.T.);
#10320=ORIENTED_EDGE('',*,*,#7498,.T.);
#10321=ORIENTED_EDGE('',*,*,#7503,.F.);
#10322=ORIENTED_EDGE('',*,*,#7504,.F.);
#10323=ORIENTED_EDGE('',*,*,#7450,.F.);
#10324=ORIENTED_EDGE('',*,*,#7486,.T.);
#10325=ORIENTED_EDGE('',*,*,#7496,.F.);
#10326=ORIENTED_EDGE('',*,*,#7501,.F.);
#10327=ORIENTED_EDGE('',*,*,#7384,.F.);
#10328=ORIENTED_EDGE('',*,*,#7392,.F.);
#10329=ORIENTED_EDGE('',*,*,#7438,.T.);
#10330=ORIENTED_EDGE('',*,*,#7408,.F.);
#10331=ORIENTED_EDGE('',*,*,#7404,.F.);
#10332=ORIENTED_EDGE('',*,*,#7443,.T.);
#10333=ORIENTED_EDGE('',*,*,#7504,.T.);
#10334=ORIENTED_EDGE('',*,*,#7505,.F.);
#10335=ORIENTED_EDGE('',*,*,#7506,.F.);
#10336=ORIENTED_EDGE('',*,*,#7378,.T.);
#10337=ORIENTED_EDGE('',*,*,#7381,.T.);
#10338=ORIENTED_EDGE('',*,*,#7499,.F.);
#10339=ORIENTED_EDGE('',*,*,#7406,.F.);
#10340=ORIENTED_EDGE('',*,*,#7414,.F.);
#10341=ORIENTED_EDGE('',*,*,#7439,.F.);
#10342=ORIENTED_EDGE('',*,*,#7386,.F.);
#10343=ORIENTED_EDGE('',*,*,#7382,.F.);
#10344=ORIENTED_EDGE('',*,*,#7502,.T.);
#10345=ORIENTED_EDGE('',*,*,#7497,.F.);
#10346=ORIENTED_EDGE('',*,*,#7487,.F.);
#10347=ORIENTED_EDGE('',*,*,#7444,.F.);
#10348=ORIENTED_EDGE('',*,*,#7506,.T.);
#10349=ORIENTED_EDGE('',*,*,#7507,.F.);
#10350=ORIENTED_EDGE('',*,*,#7500,.T.);
#10351=ORIENTED_EDGE('',*,*,#7507,.T.);
#10352=ORIENTED_EDGE('',*,*,#7505,.T.);
#10353=ORIENTED_EDGE('',*,*,#7503,.T.);
#10354=ORIENTED_EDGE('',*,*,#7508,.F.);
#10355=ORIENTED_EDGE('',*,*,#7509,.F.);
#10356=ORIENTED_EDGE('',*,*,#7510,.F.);
#10357=ORIENTED_EDGE('',*,*,#7511,.F.);
#10358=ORIENTED_EDGE('',*,*,#7512,.F.);
#10359=ORIENTED_EDGE('',*,*,#7513,.F.);
#10360=ORIENTED_EDGE('',*,*,#7514,.T.);
#10361=ORIENTED_EDGE('',*,*,#7509,.T.);
#10362=ORIENTED_EDGE('',*,*,#7515,.T.);
#10363=ORIENTED_EDGE('',*,*,#7516,.F.);
#10364=ORIENTED_EDGE('',*,*,#7517,.F.);
#10365=ORIENTED_EDGE('',*,*,#7510,.T.);
#10366=ORIENTED_EDGE('',*,*,#7517,.T.);
#10367=ORIENTED_EDGE('',*,*,#7518,.F.);
#10368=ORIENTED_EDGE('',*,*,#7519,.F.);
#10369=ORIENTED_EDGE('',*,*,#7511,.T.);
#10370=ORIENTED_EDGE('',*,*,#7519,.T.);
#10371=ORIENTED_EDGE('',*,*,#7520,.F.);
#10372=ORIENTED_EDGE('',*,*,#7521,.F.);
#10373=ORIENTED_EDGE('',*,*,#7512,.T.);
#10374=ORIENTED_EDGE('',*,*,#7521,.T.);
#10375=ORIENTED_EDGE('',*,*,#7522,.F.);
#10376=ORIENTED_EDGE('',*,*,#7523,.F.);
#10377=ORIENTED_EDGE('',*,*,#7513,.T.);
#10378=ORIENTED_EDGE('',*,*,#7523,.T.);
#10379=ORIENTED_EDGE('',*,*,#7524,.F.);
#10380=ORIENTED_EDGE('',*,*,#7525,.F.);
#10381=ORIENTED_EDGE('',*,*,#7508,.T.);
#10382=ORIENTED_EDGE('',*,*,#7525,.T.);
#10383=ORIENTED_EDGE('',*,*,#7526,.F.);
#10384=ORIENTED_EDGE('',*,*,#7515,.F.);
#10385=ORIENTED_EDGE('',*,*,#7526,.T.);
#10386=ORIENTED_EDGE('',*,*,#7524,.T.);
#10387=ORIENTED_EDGE('',*,*,#7522,.T.);
#10388=ORIENTED_EDGE('',*,*,#7520,.T.);
#10389=ORIENTED_EDGE('',*,*,#7518,.T.);
#10390=ORIENTED_EDGE('',*,*,#7516,.T.);
#10391=ORIENTED_EDGE('',*,*,#7527,.F.);
#10392=ORIENTED_EDGE('',*,*,#7528,.T.);
#10393=ORIENTED_EDGE('',*,*,#7514,.F.);
#10394=ORIENTED_EDGE('',*,*,#7528,.F.);
#10395=ORIENTED_EDGE('',*,*,#7527,.T.);
#10396=ORIENTED_EDGE('',*,*,#7529,.F.);
#10397=ORIENTED_EDGE('',*,*,#7530,.T.);
#10398=ORIENTED_EDGE('',*,*,#7531,.F.);
#10399=ORIENTED_EDGE('',*,*,#7530,.F.);
#10400=ORIENTED_EDGE('',*,*,#7532,.F.);
#10401=ORIENTED_EDGE('',*,*,#7533,.T.);
#10402=ORIENTED_EDGE('',*,*,#7534,.F.);
#10403=ORIENTED_EDGE('',*,*,#7535,.F.);
#10404=ORIENTED_EDGE('',*,*,#7536,.F.);
#10405=ORIENTED_EDGE('',*,*,#7535,.T.);
#10406=ORIENTED_EDGE('',*,*,#7537,.F.);
#10407=ORIENTED_EDGE('',*,*,#7538,.F.);
#10408=ORIENTED_EDGE('',*,*,#7539,.F.);
#10409=ORIENTED_EDGE('',*,*,#7538,.T.);
#10410=ORIENTED_EDGE('',*,*,#7540,.F.);
#10411=ORIENTED_EDGE('',*,*,#7541,.F.);
#10412=ORIENTED_EDGE('',*,*,#7542,.F.);
#10413=ORIENTED_EDGE('',*,*,#7541,.T.);
#10414=ORIENTED_EDGE('',*,*,#7543,.F.);
#10415=ORIENTED_EDGE('',*,*,#7544,.F.);
#10416=ORIENTED_EDGE('',*,*,#7545,.F.);
#10417=ORIENTED_EDGE('',*,*,#7544,.T.);
#10418=ORIENTED_EDGE('',*,*,#7546,.F.);
#10419=ORIENTED_EDGE('',*,*,#7547,.F.);
#10420=ORIENTED_EDGE('',*,*,#7548,.F.);
#10421=ORIENTED_EDGE('',*,*,#7547,.T.);
#10422=ORIENTED_EDGE('',*,*,#7549,.F.);
#10423=ORIENTED_EDGE('',*,*,#7533,.F.);
#10424=ORIENTED_EDGE('',*,*,#7548,.T.);
#10425=ORIENTED_EDGE('',*,*,#7532,.T.);
#10426=ORIENTED_EDGE('',*,*,#7536,.T.);
#10427=ORIENTED_EDGE('',*,*,#7539,.T.);
#10428=ORIENTED_EDGE('',*,*,#7542,.T.);
#10429=ORIENTED_EDGE('',*,*,#7545,.T.);
#10430=ORIENTED_EDGE('',*,*,#7531,.T.);
#10431=ORIENTED_EDGE('',*,*,#7549,.T.);
#10432=ORIENTED_EDGE('',*,*,#7546,.T.);
#10433=ORIENTED_EDGE('',*,*,#7543,.T.);
#10434=ORIENTED_EDGE('',*,*,#7540,.T.);
#10435=ORIENTED_EDGE('',*,*,#7537,.T.);
#10436=ORIENTED_EDGE('',*,*,#7534,.T.);
#10437=ORIENTED_EDGE('',*,*,#7529,.T.);
#10438=ORIENTED_EDGE('',*,*,#7550,.F.);
#10439=ORIENTED_EDGE('',*,*,#7551,.T.);
#10440=ORIENTED_EDGE('',*,*,#7552,.F.);
#10441=ORIENTED_EDGE('',*,*,#7551,.F.);
#10442=ORIENTED_EDGE('',*,*,#7553,.F.);
#10443=ORIENTED_EDGE('',*,*,#7554,.T.);
#10444=ORIENTED_EDGE('',*,*,#7555,.F.);
#10445=ORIENTED_EDGE('',*,*,#7556,.F.);
#10446=ORIENTED_EDGE('',*,*,#7557,.F.);
#10447=ORIENTED_EDGE('',*,*,#7556,.T.);
#10448=ORIENTED_EDGE('',*,*,#7558,.F.);
#10449=ORIENTED_EDGE('',*,*,#7559,.F.);
#10450=ORIENTED_EDGE('',*,*,#7560,.F.);
#10451=ORIENTED_EDGE('',*,*,#7559,.T.);
#10452=ORIENTED_EDGE('',*,*,#7561,.F.);
#10453=ORIENTED_EDGE('',*,*,#7562,.F.);
#10454=ORIENTED_EDGE('',*,*,#7563,.F.);
#10455=ORIENTED_EDGE('',*,*,#7562,.T.);
#10456=ORIENTED_EDGE('',*,*,#7564,.F.);
#10457=ORIENTED_EDGE('',*,*,#7565,.F.);
#10458=ORIENTED_EDGE('',*,*,#7566,.F.);
#10459=ORIENTED_EDGE('',*,*,#7565,.T.);
#10460=ORIENTED_EDGE('',*,*,#7567,.F.);
#10461=ORIENTED_EDGE('',*,*,#7568,.F.);
#10462=ORIENTED_EDGE('',*,*,#7569,.F.);
#10463=ORIENTED_EDGE('',*,*,#7568,.T.);
#10464=ORIENTED_EDGE('',*,*,#7570,.F.);
#10465=ORIENTED_EDGE('',*,*,#7554,.F.);
#10466=ORIENTED_EDGE('',*,*,#7569,.T.);
#10467=ORIENTED_EDGE('',*,*,#7553,.T.);
#10468=ORIENTED_EDGE('',*,*,#7557,.T.);
#10469=ORIENTED_EDGE('',*,*,#7560,.T.);
#10470=ORIENTED_EDGE('',*,*,#7563,.T.);
#10471=ORIENTED_EDGE('',*,*,#7566,.T.);
#10472=ORIENTED_EDGE('',*,*,#7552,.T.);
#10473=ORIENTED_EDGE('',*,*,#7570,.T.);
#10474=ORIENTED_EDGE('',*,*,#7567,.T.);
#10475=ORIENTED_EDGE('',*,*,#7564,.T.);
#10476=ORIENTED_EDGE('',*,*,#7561,.T.);
#10477=ORIENTED_EDGE('',*,*,#7558,.T.);
#10478=ORIENTED_EDGE('',*,*,#7555,.T.);
#10479=ORIENTED_EDGE('',*,*,#7550,.T.);
#10480=ORIENTED_EDGE('',*,*,#7571,.T.);
#10481=ORIENTED_EDGE('',*,*,#7572,.T.);
#10482=ORIENTED_EDGE('',*,*,#7573,.T.);
#10483=ORIENTED_EDGE('',*,*,#7574,.F.);
#10484=ORIENTED_EDGE('',*,*,#7575,.F.);
#10485=ORIENTED_EDGE('',*,*,#7576,.T.);
#10486=ORIENTED_EDGE('',*,*,#7577,.T.);
#10487=ORIENTED_EDGE('',*,*,#7572,.F.);
#10488=ORIENTED_EDGE('',*,*,#7578,.T.);
#10489=ORIENTED_EDGE('',*,*,#7579,.F.);
#10490=ORIENTED_EDGE('',*,*,#7580,.T.);
#10491=ORIENTED_EDGE('',*,*,#7576,.F.);
#10492=ORIENTED_EDGE('',*,*,#7581,.F.);
#10493=ORIENTED_EDGE('',*,*,#7582,.T.);
#10494=ORIENTED_EDGE('',*,*,#7583,.T.);
#10495=ORIENTED_EDGE('',*,*,#7584,.F.);
#10496=ORIENTED_EDGE('',*,*,#7585,.T.);
#10497=ORIENTED_EDGE('',*,*,#7586,.T.);
#10498=ORIENTED_EDGE('',*,*,#7587,.T.);
#10499=ORIENTED_EDGE('',*,*,#7582,.F.);
#10500=ORIENTED_EDGE('',*,*,#7588,.F.);
#10501=ORIENTED_EDGE('',*,*,#7589,.T.);
#10502=ORIENTED_EDGE('',*,*,#7590,.T.);
#10503=ORIENTED_EDGE('',*,*,#7586,.F.);
#10504=ORIENTED_EDGE('',*,*,#7591,.F.);
#10505=ORIENTED_EDGE('',*,*,#7592,.T.);
#10506=ORIENTED_EDGE('',*,*,#7593,.T.);
#10507=ORIENTED_EDGE('',*,*,#7589,.F.);
#10508=ORIENTED_EDGE('',*,*,#7594,.T.);
#10509=ORIENTED_EDGE('',*,*,#7574,.T.);
#10510=ORIENTED_EDGE('',*,*,#7595,.T.);
#10511=ORIENTED_EDGE('',*,*,#7596,.F.);
#10512=ORIENTED_EDGE('',*,*,#7597,.T.);
#10513=ORIENTED_EDGE('',*,*,#7598,.T.);
#10514=ORIENTED_EDGE('',*,*,#7599,.T.);
#10515=ORIENTED_EDGE('',*,*,#7592,.F.);
#10516=ORIENTED_EDGE('',*,*,#7600,.F.);
#10517=ORIENTED_EDGE('',*,*,#7601,.T.);
#10518=ORIENTED_EDGE('',*,*,#7602,.F.);
#10519=ORIENTED_EDGE('',*,*,#7603,.F.);
#10520=ORIENTED_EDGE('',*,*,#7604,.T.);
#10521=ORIENTED_EDGE('',*,*,#7603,.T.);
#10522=ORIENTED_EDGE('',*,*,#7605,.F.);
#10523=ORIENTED_EDGE('',*,*,#7606,.F.);
#10524=ORIENTED_EDGE('',*,*,#7607,.F.);
#10525=ORIENTED_EDGE('',*,*,#7606,.T.);
#10526=ORIENTED_EDGE('',*,*,#7608,.F.);
#10527=ORIENTED_EDGE('',*,*,#7609,.F.);
#10528=ORIENTED_EDGE('',*,*,#7610,.T.);
#10529=ORIENTED_EDGE('',*,*,#7611,.F.);
#10530=ORIENTED_EDGE('',*,*,#7612,.F.);
#10531=ORIENTED_EDGE('',*,*,#7613,.F.);
#10532=ORIENTED_EDGE('',*,*,#7614,.F.);
#10533=ORIENTED_EDGE('',*,*,#7613,.T.);
#10534=ORIENTED_EDGE('',*,*,#7615,.F.);
#10535=ORIENTED_EDGE('',*,*,#7616,.F.);
#10536=ORIENTED_EDGE('',*,*,#7617,.T.);
#10537=ORIENTED_EDGE('',*,*,#7616,.T.);
#10538=ORIENTED_EDGE('',*,*,#7618,.F.);
#10539=ORIENTED_EDGE('',*,*,#7619,.F.);
#10540=ORIENTED_EDGE('',*,*,#7620,.T.);
#10541=ORIENTED_EDGE('',*,*,#7619,.T.);
#10542=ORIENTED_EDGE('',*,*,#7621,.F.);
#10543=ORIENTED_EDGE('',*,*,#7598,.F.);
#10544=ORIENTED_EDGE('',*,*,#7622,.F.);
#10545=ORIENTED_EDGE('',*,*,#7623,.F.);
#10546=ORIENTED_EDGE('',*,*,#7624,.F.);
#10547=ORIENTED_EDGE('',*,*,#7596,.T.);
#10548=ORIENTED_EDGE('',*,*,#7625,.F.);
#10549=ORIENTED_EDGE('',*,*,#7623,.T.);
#10550=ORIENTED_EDGE('',*,*,#7626,.F.);
#10551=ORIENTED_EDGE('',*,*,#7601,.F.);
#10552=ORIENTED_EDGE('',*,*,#7609,.T.);
#10553=ORIENTED_EDGE('',*,*,#7627,.F.);
#10554=ORIENTED_EDGE('',*,*,#7628,.F.);
#10555=ORIENTED_EDGE('',*,*,#7629,.T.);
#10556=ORIENTED_EDGE('',*,*,#7579,.T.);
#10557=ORIENTED_EDGE('',*,*,#7630,.T.);
#10558=ORIENTED_EDGE('',*,*,#7631,.T.);
#10559=ORIENTED_EDGE('',*,*,#7632,.F.);
#10560=ORIENTED_EDGE('',*,*,#7584,.T.);
#10561=ORIENTED_EDGE('',*,*,#7633,.F.);
#10562=ORIENTED_EDGE('',*,*,#7611,.T.);
#10563=ORIENTED_EDGE('',*,*,#7634,.T.);
#10564=ORIENTED_EDGE('',*,*,#7635,.F.);
#10565=ORIENTED_EDGE('',*,*,#7636,.T.);
#10566=ORIENTED_EDGE('',*,*,#7637,.T.);
#10567=ORIENTED_EDGE('',*,*,#7631,.F.);
#10568=ORIENTED_EDGE('',*,*,#7638,.T.);
#10569=ORIENTED_EDGE('',*,*,#7639,.T.);
#10570=ORIENTED_EDGE('',*,*,#7640,.T.);
#10571=ORIENTED_EDGE('',*,*,#7636,.F.);
#10572=ORIENTED_EDGE('',*,*,#7641,.F.);
#10573=ORIENTED_EDGE('',*,*,#7642,.T.);
#10574=ORIENTED_EDGE('',*,*,#7643,.T.);
#10575=ORIENTED_EDGE('',*,*,#7639,.F.);
#10576=ORIENTED_EDGE('',*,*,#7644,.T.);
#10577=ORIENTED_EDGE('',*,*,#7645,.T.);
#10578=ORIENTED_EDGE('',*,*,#7646,.T.);
#10579=ORIENTED_EDGE('',*,*,#7642,.F.);
#10580=ORIENTED_EDGE('',*,*,#7647,.F.);
#10581=ORIENTED_EDGE('',*,*,#7648,.T.);
#10582=ORIENTED_EDGE('',*,*,#7649,.T.);
#10583=ORIENTED_EDGE('',*,*,#7645,.F.);
#10584=ORIENTED_EDGE('',*,*,#7650,.F.);
#10585=ORIENTED_EDGE('',*,*,#7651,.T.);
#10586=ORIENTED_EDGE('',*,*,#7652,.T.);
#10587=ORIENTED_EDGE('',*,*,#7648,.F.);
#10588=ORIENTED_EDGE('',*,*,#7653,.T.);
#10589=ORIENTED_EDGE('',*,*,#7654,.T.);
#10590=ORIENTED_EDGE('',*,*,#7655,.T.);
#10591=ORIENTED_EDGE('',*,*,#7651,.F.);
#10592=ORIENTED_EDGE('',*,*,#7656,.F.);
#10593=ORIENTED_EDGE('',*,*,#7657,.T.);
#10594=ORIENTED_EDGE('',*,*,#7658,.T.);
#10595=ORIENTED_EDGE('',*,*,#7654,.F.);
#10596=ORIENTED_EDGE('',*,*,#7659,.T.);
#10597=ORIENTED_EDGE('',*,*,#7660,.T.);
#10598=ORIENTED_EDGE('',*,*,#7661,.T.);
#10599=ORIENTED_EDGE('',*,*,#7657,.F.);
#10600=ORIENTED_EDGE('',*,*,#7662,.T.);
#10601=ORIENTED_EDGE('',*,*,#7663,.T.);
#10602=ORIENTED_EDGE('',*,*,#7664,.T.);
#10603=ORIENTED_EDGE('',*,*,#7660,.F.);
#10604=ORIENTED_EDGE('',*,*,#7665,.T.);
#10605=ORIENTED_EDGE('',*,*,#7628,.T.);
#10606=ORIENTED_EDGE('',*,*,#7666,.F.);
#10607=ORIENTED_EDGE('',*,*,#7667,.F.);
#10608=ORIENTED_EDGE('',*,*,#7668,.F.);
#10609=ORIENTED_EDGE('',*,*,#7667,.T.);
#10610=ORIENTED_EDGE('',*,*,#7669,.F.);
#10611=ORIENTED_EDGE('',*,*,#7670,.F.);
#10612=ORIENTED_EDGE('',*,*,#7671,.T.);
#10613=ORIENTED_EDGE('',*,*,#7670,.T.);
#10614=ORIENTED_EDGE('',*,*,#7672,.F.);
#10615=ORIENTED_EDGE('',*,*,#7673,.F.);
#10616=ORIENTED_EDGE('',*,*,#7674,.F.);
#10617=ORIENTED_EDGE('',*,*,#7673,.T.);
#10618=ORIENTED_EDGE('',*,*,#7675,.F.);
#10619=ORIENTED_EDGE('',*,*,#7676,.F.);
#10620=ORIENTED_EDGE('',*,*,#7677,.T.);
#10621=ORIENTED_EDGE('',*,*,#7676,.T.);
#10622=ORIENTED_EDGE('',*,*,#7678,.F.);
#10623=ORIENTED_EDGE('',*,*,#7679,.F.);
#10624=ORIENTED_EDGE('',*,*,#7680,.T.);
#10625=ORIENTED_EDGE('',*,*,#7679,.T.);
#10626=ORIENTED_EDGE('',*,*,#7681,.F.);
#10627=ORIENTED_EDGE('',*,*,#7682,.F.);
#10628=ORIENTED_EDGE('',*,*,#7683,.F.);
#10629=ORIENTED_EDGE('',*,*,#7682,.T.);
#10630=ORIENTED_EDGE('',*,*,#7684,.F.);
#10631=ORIENTED_EDGE('',*,*,#7685,.F.);
#10632=ORIENTED_EDGE('',*,*,#7686,.T.);
#10633=ORIENTED_EDGE('',*,*,#7685,.T.);
#10634=ORIENTED_EDGE('',*,*,#7687,.F.);
#10635=ORIENTED_EDGE('',*,*,#7688,.F.);
#10636=ORIENTED_EDGE('',*,*,#7689,.F.);
#10637=ORIENTED_EDGE('',*,*,#7688,.T.);
#10638=ORIENTED_EDGE('',*,*,#7690,.F.);
#10639=ORIENTED_EDGE('',*,*,#7663,.F.);
#10640=ORIENTED_EDGE('',*,*,#7578,.F.);
#10641=ORIENTED_EDGE('',*,*,#7575,.T.);
#10642=ORIENTED_EDGE('',*,*,#7571,.F.);
#10643=ORIENTED_EDGE('',*,*,#7594,.F.);
#10644=ORIENTED_EDGE('',*,*,#7624,.T.);
#10645=ORIENTED_EDGE('',*,*,#7625,.T.);
#10646=ORIENTED_EDGE('',*,*,#7600,.T.);
#10647=ORIENTED_EDGE('',*,*,#7604,.F.);
#10648=ORIENTED_EDGE('',*,*,#7607,.T.);
#10649=ORIENTED_EDGE('',*,*,#7629,.F.);
#10650=ORIENTED_EDGE('',*,*,#7665,.F.);
#10651=ORIENTED_EDGE('',*,*,#7668,.T.);
#10652=ORIENTED_EDGE('',*,*,#7671,.F.);
#10653=ORIENTED_EDGE('',*,*,#7674,.T.);
#10654=ORIENTED_EDGE('',*,*,#7677,.F.);
#10655=ORIENTED_EDGE('',*,*,#7680,.F.);
#10656=ORIENTED_EDGE('',*,*,#7683,.T.);
#10657=ORIENTED_EDGE('',*,*,#7686,.F.);
#10658=ORIENTED_EDGE('',*,*,#7689,.T.);
#10659=ORIENTED_EDGE('',*,*,#7662,.F.);
#10660=ORIENTED_EDGE('',*,*,#7659,.F.);
#10661=ORIENTED_EDGE('',*,*,#7656,.T.);
#10662=ORIENTED_EDGE('',*,*,#7653,.F.);
#10663=ORIENTED_EDGE('',*,*,#7650,.T.);
#10664=ORIENTED_EDGE('',*,*,#7647,.T.);
#10665=ORIENTED_EDGE('',*,*,#7644,.F.);
#10666=ORIENTED_EDGE('',*,*,#7641,.T.);
#10667=ORIENTED_EDGE('',*,*,#7638,.F.);
#10668=ORIENTED_EDGE('',*,*,#7635,.T.);
#10669=ORIENTED_EDGE('',*,*,#7630,.F.);
#10670=ORIENTED_EDGE('',*,*,#7634,.F.);
#10671=ORIENTED_EDGE('',*,*,#7610,.F.);
#10672=ORIENTED_EDGE('',*,*,#7614,.T.);
#10673=ORIENTED_EDGE('',*,*,#7617,.F.);
#10674=ORIENTED_EDGE('',*,*,#7620,.F.);
#10675=ORIENTED_EDGE('',*,*,#7597,.F.);
#10676=ORIENTED_EDGE('',*,*,#7591,.T.);
#10677=ORIENTED_EDGE('',*,*,#7588,.T.);
#10678=ORIENTED_EDGE('',*,*,#7585,.F.);
#10679=ORIENTED_EDGE('',*,*,#7581,.T.);
#10680=ORIENTED_EDGE('',*,*,#7632,.T.);
#10681=ORIENTED_EDGE('',*,*,#7637,.F.);
#10682=ORIENTED_EDGE('',*,*,#7640,.F.);
#10683=ORIENTED_EDGE('',*,*,#7643,.F.);
#10684=ORIENTED_EDGE('',*,*,#7646,.F.);
#10685=ORIENTED_EDGE('',*,*,#7649,.F.);
#10686=ORIENTED_EDGE('',*,*,#7652,.F.);
#10687=ORIENTED_EDGE('',*,*,#7655,.F.);
#10688=ORIENTED_EDGE('',*,*,#7658,.F.);
#10689=ORIENTED_EDGE('',*,*,#7661,.F.);
#10690=ORIENTED_EDGE('',*,*,#7664,.F.);
#10691=ORIENTED_EDGE('',*,*,#7690,.T.);
#10692=ORIENTED_EDGE('',*,*,#7687,.T.);
#10693=ORIENTED_EDGE('',*,*,#7684,.T.);
#10694=ORIENTED_EDGE('',*,*,#7681,.T.);
#10695=ORIENTED_EDGE('',*,*,#7678,.T.);
#10696=ORIENTED_EDGE('',*,*,#7675,.T.);
#10697=ORIENTED_EDGE('',*,*,#7672,.T.);
#10698=ORIENTED_EDGE('',*,*,#7669,.T.);
#10699=ORIENTED_EDGE('',*,*,#7666,.T.);
#10700=ORIENTED_EDGE('',*,*,#7627,.T.);
#10701=ORIENTED_EDGE('',*,*,#7608,.T.);
#10702=ORIENTED_EDGE('',*,*,#7605,.T.);
#10703=ORIENTED_EDGE('',*,*,#7602,.T.);
#10704=ORIENTED_EDGE('',*,*,#7626,.T.);
#10705=ORIENTED_EDGE('',*,*,#7622,.T.);
#10706=ORIENTED_EDGE('',*,*,#7595,.F.);
#10707=ORIENTED_EDGE('',*,*,#7573,.F.);
#10708=ORIENTED_EDGE('',*,*,#7577,.F.);
#10709=ORIENTED_EDGE('',*,*,#7580,.F.);
#10710=ORIENTED_EDGE('',*,*,#7583,.F.);
#10711=ORIENTED_EDGE('',*,*,#7587,.F.);
#10712=ORIENTED_EDGE('',*,*,#7590,.F.);
#10713=ORIENTED_EDGE('',*,*,#7593,.F.);
#10714=ORIENTED_EDGE('',*,*,#7599,.F.);
#10715=ORIENTED_EDGE('',*,*,#7621,.T.);
#10716=ORIENTED_EDGE('',*,*,#7618,.T.);
#10717=ORIENTED_EDGE('',*,*,#7615,.T.);
#10718=ORIENTED_EDGE('',*,*,#7612,.T.);
#10719=ORIENTED_EDGE('',*,*,#7633,.T.);
#10720=ORIENTED_EDGE('',*,*,#7691,.F.);
#10721=ORIENTED_EDGE('',*,*,#7692,.T.);
#10722=ORIENTED_EDGE('',*,*,#7693,.F.);
#10723=ORIENTED_EDGE('',*,*,#7692,.F.);
#10724=ORIENTED_EDGE('',*,*,#7694,.F.);
#10725=ORIENTED_EDGE('',*,*,#7695,.T.);
#10726=ORIENTED_EDGE('',*,*,#7696,.F.);
#10727=ORIENTED_EDGE('',*,*,#7697,.F.);
#10728=ORIENTED_EDGE('',*,*,#7698,.F.);
#10729=ORIENTED_EDGE('',*,*,#7697,.T.);
#10730=ORIENTED_EDGE('',*,*,#7699,.F.);
#10731=ORIENTED_EDGE('',*,*,#7700,.F.);
#10732=ORIENTED_EDGE('',*,*,#7701,.F.);
#10733=ORIENTED_EDGE('',*,*,#7700,.T.);
#10734=ORIENTED_EDGE('',*,*,#7702,.F.);
#10735=ORIENTED_EDGE('',*,*,#7703,.F.);
#10736=ORIENTED_EDGE('',*,*,#7704,.F.);
#10737=ORIENTED_EDGE('',*,*,#7703,.T.);
#10738=ORIENTED_EDGE('',*,*,#7705,.F.);
#10739=ORIENTED_EDGE('',*,*,#7706,.F.);
#10740=ORIENTED_EDGE('',*,*,#7707,.F.);
#10741=ORIENTED_EDGE('',*,*,#7706,.T.);
#10742=ORIENTED_EDGE('',*,*,#7708,.F.);
#10743=ORIENTED_EDGE('',*,*,#7709,.F.);
#10744=ORIENTED_EDGE('',*,*,#7710,.F.);
#10745=ORIENTED_EDGE('',*,*,#7709,.T.);
#10746=ORIENTED_EDGE('',*,*,#7711,.F.);
#10747=ORIENTED_EDGE('',*,*,#7695,.F.);
#10748=ORIENTED_EDGE('',*,*,#7710,.T.);
#10749=ORIENTED_EDGE('',*,*,#7694,.T.);
#10750=ORIENTED_EDGE('',*,*,#7698,.T.);
#10751=ORIENTED_EDGE('',*,*,#7701,.T.);
#10752=ORIENTED_EDGE('',*,*,#7704,.T.);
#10753=ORIENTED_EDGE('',*,*,#7707,.T.);
#10754=ORIENTED_EDGE('',*,*,#7693,.T.);
#10755=ORIENTED_EDGE('',*,*,#7711,.T.);
#10756=ORIENTED_EDGE('',*,*,#7708,.T.);
#10757=ORIENTED_EDGE('',*,*,#7705,.T.);
#10758=ORIENTED_EDGE('',*,*,#7702,.T.);
#10759=ORIENTED_EDGE('',*,*,#7699,.T.);
#10760=ORIENTED_EDGE('',*,*,#7696,.T.);
#10761=ORIENTED_EDGE('',*,*,#7691,.T.);
#10762=TOROIDAL_SURFACE('',#11485,20.7480593298244,0.5);
#10763=TOROIDAL_SURFACE('',#11494,20.7480593298244,0.5);
#10764=TOROIDAL_SURFACE('',#11497,20.7480593298244,0.5);
#10765=TOROIDAL_SURFACE('',#11505,20.7480593298244,0.5);
#10766=TOROIDAL_SURFACE('',#11511,20.7480593298244,0.5);
#10767=TOROIDAL_SURFACE('',#11520,20.7480593298244,0.5);
#10768=ADVANCED_FACE('',(#2892),#10762,.T.);
#10769=ADVANCED_FACE('',(#2893),#2549,.T.);
#10770=ADVANCED_FACE('',(#2894),#626,.T.);
#10771=ADVANCED_FACE('',(#2895),#10763,.T.);
#10772=ADVANCED_FACE('',(#2896),#10764,.T.);
#10773=ADVANCED_FACE('',(#2897),#2550,.T.);
#10774=ADVANCED_FACE('',(#2898),#10765,.T.);
#10775=ADVANCED_FACE('',(#2899),#627,.T.);
#10776=ADVANCED_FACE('',(#2900),#2551,.T.);
#10777=ADVANCED_FACE('',(#2901),#10766,.T.);
#10778=ADVANCED_FACE('',(#2902),#2552,.T.);
#10779=ADVANCED_FACE('',(#2903,#109),#628,.T.);
#10780=ADVANCED_FACE('',(#2904),#10767,.T.);
#10781=ADVANCED_FACE('',(#2905,#110),#629,.T.);
#10782=ADVANCED_FACE('',(#2906),#2553,.T.);
#10783=ADVANCED_FACE('',(#2907,#111),#630,.F.);
#10784=ADVANCED_FACE('',(#2908,#112),#631,.T.);
#10785=ADVANCED_FACE('',(#2909,#113),#632,.F.);
#10786=ADVANCED_FACE('',(#2910),#2554,.T.);
#10787=ADVANCED_FACE('',(#2911),#2555,.T.);
#10788=ADVANCED_FACE('',(#2912,#114),#633,.F.);
#10789=ADVANCED_FACE('',(#2913),#2556,.T.);
#10790=ADVANCED_FACE('',(#2914,#115),#634,.T.);
#10791=ADVANCED_FACE('',(#2915),#2557,.F.);
#10792=ADVANCED_FACE('',(#2916),#2558,.F.);
#10793=ADVANCED_FACE('',(#2917),#2559,.T.);
#10794=ADVANCED_FACE('',(#2918,#116),#635,.T.);
#10795=ADVANCED_FACE('',(#2919),#2560,.F.);
#10796=ADVANCED_FACE('',(#2920,#117),#636,.F.);
#10797=ADVANCED_FACE('',(#2921),#2561,.T.);
#10798=ADVANCED_FACE('',(#2922,#118,#119,#120,#121,#122,#123,#124,#125,
#126,#127,#128),#637,.T.);
#10799=ADVANCED_FACE('',(#2923),#638,.F.);
#10800=ADVANCED_FACE('',(#2924),#2562,.T.);
#10801=ADVANCED_FACE('',(#2925),#2563,.F.);
#10802=ADVANCED_FACE('',(#2926),#2564,.F.);
#10803=ADVANCED_FACE('',(#2927),#2565,.F.);
#10804=ADVANCED_FACE('',(#2928),#2566,.F.);
#10805=ADVANCED_FACE('',(#2929),#2567,.F.);
#10806=ADVANCED_FACE('',(#2930),#2568,.F.);
#10807=ADVANCED_FACE('',(#2931),#2569,.F.);
#10808=ADVANCED_FACE('',(#2932),#2570,.F.);
#10809=ADVANCED_FACE('',(#2933),#2571,.F.);
#10810=ADVANCED_FACE('',(#2934),#2572,.F.);
#10811=ADVANCED_FACE('',(#2935),#2573,.F.);
#10812=ADVANCED_FACE('',(#2936),#2574,.F.);
#10813=ADVANCED_FACE('',(#2937),#2575,.F.);
#10814=ADVANCED_FACE('',(#2938),#2576,.F.);
#10815=ADVANCED_FACE('',(#2939),#2577,.F.);
#10816=ADVANCED_FACE('',(#2940),#2578,.F.);
#10817=ADVANCED_FACE('',(#2941),#2579,.F.);
#10818=ADVANCED_FACE('',(#2942),#2580,.F.);
#10819=ADVANCED_FACE('',(#2943),#2581,.F.);
#10820=ADVANCED_FACE('',(#2944),#2582,.F.);
#10821=ADVANCED_FACE('',(#2945),#2583,.F.);
#10822=ADVANCED_FACE('',(#2946),#2584,.F.);
#10823=ADVANCED_FACE('',(#2947),#2585,.F.);
#10824=ADVANCED_FACE('',(#2948),#2586,.F.);
#10825=ADVANCED_FACE('',(#2949),#2587,.F.);
#10826=ADVANCED_FACE('',(#2950),#2588,.F.);
#10827=ADVANCED_FACE('',(#2951),#2589,.F.);
#10828=ADVANCED_FACE('',(#2952),#2590,.F.);
#10829=ADVANCED_FACE('',(#2953),#2591,.F.);
#10830=ADVANCED_FACE('',(#2954),#2592,.F.);
#10831=ADVANCED_FACE('',(#2955),#2593,.F.);
#10832=ADVANCED_FACE('',(#2956),#2594,.F.);
#10833=ADVANCED_FACE('',(#2957),#2595,.F.);
#10834=ADVANCED_FACE('',(#2958),#639,.T.);
#10835=ADVANCED_FACE('',(#2959,#129,#130,#131,#132,#133,#134,#135,#136,
#137,#138,#139),#640,.T.);
#10836=ADVANCED_FACE('',(#2960,#140,#141,#142,#143,#144,#145,#146,#147,
#148,#149,#150),#641,.T.);
#10837=ADVANCED_FACE('',(#2961),#642,.T.);
#10838=ADVANCED_FACE('',(#2962,#151,#152,#153,#154,#155,#156,#157,#158,
#159,#160,#161),#643,.T.);
#10839=ADVANCED_FACE('',(#2963,#162,#163,#164,#165,#166,#167,#168,#169,
#170,#171,#172),#644,.T.);
#10840=ADVANCED_FACE('',(#2964,#173,#174,#175,#176,#177,#178,#179,#180,
#181,#182,#183),#645,.T.);
#10841=ADVANCED_FACE('',(#2965),#646,.T.);
#10842=ADVANCED_FACE('',(#2966,#184),#647,.F.);
#10843=ADVANCED_FACE('',(#2967),#648,.T.);
#10844=ADVANCED_FACE('',(#2968),#649,.T.);
#10845=ADVANCED_FACE('',(#2969),#650,.T.);
#10846=ADVANCED_FACE('',(#2970),#651,.T.);
#10847=ADVANCED_FACE('',(#2971),#652,.T.);
#10848=ADVANCED_FACE('',(#2972),#653,.T.);
#10849=ADVANCED_FACE('',(#2973),#654,.T.);
#10850=ADVANCED_FACE('',(#2974),#2596,.T.);
#10851=ADVANCED_FACE('',(#2975),#655,.F.);
#10852=ADVANCED_FACE('',(#2976),#656,.F.);
#10853=ADVANCED_FACE('',(#2977),#2597,.F.);
#10854=ADVANCED_FACE('',(#2978),#657,.F.);
#10855=ADVANCED_FACE('',(#2979),#658,.F.);
#10856=ADVANCED_FACE('',(#2980),#2598,.T.);
#10857=ADVANCED_FACE('',(#2981),#659,.F.);
#10858=ADVANCED_FACE('',(#2982),#2599,.F.);
#10859=ADVANCED_FACE('',(#2983),#2600,.T.);
#10860=ADVANCED_FACE('',(#2984),#660,.T.);
#10861=ADVANCED_FACE('',(#2985),#661,.T.);
#10862=ADVANCED_FACE('',(#2986),#2601,.F.);
#10863=ADVANCED_FACE('',(#2987),#662,.T.);
#10864=ADVANCED_FACE('',(#2988),#663,.T.);
#10865=ADVANCED_FACE('',(#2989),#2602,.T.);
#10866=ADVANCED_FACE('',(#2990),#664,.T.);
#10867=ADVANCED_FACE('',(#2991),#2603,.F.);
#10868=ADVANCED_FACE('',(#2992),#665,.T.);
#10869=ADVANCED_FACE('',(#2993),#2604,.T.);
#10870=ADVANCED_FACE('',(#2994),#666,.T.);
#10871=ADVANCED_FACE('',(#2995),#667,.T.);
#10872=ADVANCED_FACE('',(#2996),#668,.T.);
#10873=ADVANCED_FACE('',(#2997),#2605,.F.);
#10874=ADVANCED_FACE('',(#2998),#669,.F.);
#10875=ADVANCED_FACE('',(#2999),#2606,.F.);
#10876=ADVANCED_FACE('',(#3000),#670,.F.);
#10877=ADVANCED_FACE('',(#3001),#671,.F.);
#10878=ADVANCED_FACE('',(#3002),#672,.F.);
#10879=ADVANCED_FACE('',(#3003),#2607,.T.);
#10880=ADVANCED_FACE('',(#3004),#673,.F.);
#10881=ADVANCED_FACE('',(#3005),#2608,.T.);
#10882=ADVANCED_FACE('',(#3006),#674,.T.);
#10883=ADVANCED_FACE('',(#3007),#2609,.F.);
#10884=ADVANCED_FACE('',(#3008),#675,.T.);
#10885=ADVANCED_FACE('',(#3009),#2610,.F.);
#10886=ADVANCED_FACE('',(#3010),#676,.T.);
#10887=ADVANCED_FACE('',(#3011),#677,.T.);
#10888=ADVANCED_FACE('',(#3012),#678,.T.);
#10889=ADVANCED_FACE('',(#3013),#2611,.T.);
#10890=ADVANCED_FACE('',(#3014),#679,.T.);
#10891=ADVANCED_FACE('',(#3015),#2612,.T.);
#10892=ADVANCED_FACE('',(#3016,#185),#680,.T.);
#10893=ADVANCED_FACE('',(#3017,#186),#681,.F.);
#10894=ADVANCED_FACE('',(#3018),#2613,.F.);
#10895=ADVANCED_FACE('',(#3019),#2614,.F.);
#10896=ADVANCED_FACE('',(#3020),#2615,.F.);
#10897=ADVANCED_FACE('',(#3021),#2616,.F.);
#10898=ADVANCED_FACE('',(#3022),#2617,.F.);
#10899=ADVANCED_FACE('',(#3023),#682,.F.);
#10900=ADVANCED_FACE('',(#3024),#2618,.F.);
#10901=ADVANCED_FACE('',(#3025),#683,.F.);
#10902=ADVANCED_FACE('',(#3026),#2619,.F.);
#10903=ADVANCED_FACE('',(#3027),#684,.F.);
#10904=ADVANCED_FACE('',(#3028),#2620,.F.);
#10905=ADVANCED_FACE('',(#3029),#685,.F.);
#10906=ADVANCED_FACE('',(#3030),#2621,.F.);
#10907=ADVANCED_FACE('',(#3031),#2622,.F.);
#10908=ADVANCED_FACE('',(#3032),#2623,.F.);
#10909=ADVANCED_FACE('',(#3033),#2624,.F.);
#10910=ADVANCED_FACE('',(#3034),#2625,.F.);
#10911=ADVANCED_FACE('',(#3035),#2626,.F.);
#10912=ADVANCED_FACE('',(#3036),#686,.F.);
#10913=ADVANCED_FACE('',(#3037),#2627,.F.);
#10914=ADVANCED_FACE('',(#3038),#687,.F.);
#10915=ADVANCED_FACE('',(#3039),#2628,.F.);
#10916=ADVANCED_FACE('',(#3040),#688,.F.);
#10917=ADVANCED_FACE('',(#3041),#2629,.F.);
#10918=ADVANCED_FACE('',(#3042),#689,.F.);
#10919=ADVANCED_FACE('',(#3043),#2630,.F.);
#10920=ADVANCED_FACE('',(#3044),#2631,.F.);
#10921=ADVANCED_FACE('',(#3045),#2632,.F.);
#10922=ADVANCED_FACE('',(#3046),#2633,.F.);
#10923=ADVANCED_FACE('',(#3047),#2634,.F.);
#10924=ADVANCED_FACE('',(#3048),#2635,.F.);
#10925=ADVANCED_FACE('',(#3049),#690,.F.);
#10926=ADVANCED_FACE('',(#3050),#2636,.F.);
#10927=ADVANCED_FACE('',(#3051),#691,.F.);
#10928=ADVANCED_FACE('',(#3052),#2637,.F.);
#10929=ADVANCED_FACE('',(#3053),#692,.F.);
#10930=ADVANCED_FACE('',(#3054),#2638,.F.);
#10931=ADVANCED_FACE('',(#3055),#693,.F.);
#10932=ADVANCED_FACE('',(#3056),#2639,.F.);
#10933=ADVANCED_FACE('',(#3057),#2640,.F.);
#10934=ADVANCED_FACE('',(#3058),#2641,.F.);
#10935=ADVANCED_FACE('',(#3059),#2642,.F.);
#10936=ADVANCED_FACE('',(#3060),#2643,.F.);
#10937=ADVANCED_FACE('',(#3061),#2644,.F.);
#10938=ADVANCED_FACE('',(#3062),#694,.F.);
#10939=ADVANCED_FACE('',(#3063),#2645,.F.);
#10940=ADVANCED_FACE('',(#3064),#695,.F.);
#10941=ADVANCED_FACE('',(#3065),#2646,.F.);
#10942=ADVANCED_FACE('',(#3066),#696,.F.);
#10943=ADVANCED_FACE('',(#3067),#2647,.F.);
#10944=ADVANCED_FACE('',(#3068),#697,.F.);
#10945=ADVANCED_FACE('',(#3069),#2648,.F.);
#10946=ADVANCED_FACE('',(#3070),#2649,.F.);
#10947=ADVANCED_FACE('',(#3071),#2650,.F.);
#10948=ADVANCED_FACE('',(#3072),#2651,.F.);
#10949=ADVANCED_FACE('',(#3073),#2652,.F.);
#10950=ADVANCED_FACE('',(#3074),#2653,.F.);
#10951=ADVANCED_FACE('',(#3075),#698,.F.);
#10952=ADVANCED_FACE('',(#3076),#2654,.F.);
#10953=ADVANCED_FACE('',(#3077),#699,.F.);
#10954=ADVANCED_FACE('',(#3078),#2655,.F.);
#10955=ADVANCED_FACE('',(#3079),#700,.F.);
#10956=ADVANCED_FACE('',(#3080),#2656,.F.);
#10957=ADVANCED_FACE('',(#3081),#701,.F.);
#10958=ADVANCED_FACE('',(#3082),#2657,.F.);
#10959=ADVANCED_FACE('',(#3083),#2658,.F.);
#10960=ADVANCED_FACE('',(#3084),#2659,.F.);
#10961=ADVANCED_FACE('',(#3085),#2660,.F.);
#10962=ADVANCED_FACE('',(#3086),#2661,.F.);
#10963=ADVANCED_FACE('',(#3087),#2662,.F.);
#10964=ADVANCED_FACE('',(#3088),#702,.F.);
#10965=ADVANCED_FACE('',(#3089),#2663,.F.);
#10966=ADVANCED_FACE('',(#3090),#703,.F.);
#10967=ADVANCED_FACE('',(#3091),#2664,.F.);
#10968=ADVANCED_FACE('',(#3092),#704,.F.);
#10969=ADVANCED_FACE('',(#3093),#2665,.F.);
#10970=ADVANCED_FACE('',(#3094),#705,.F.);
#10971=ADVANCED_FACE('',(#3095),#2666,.F.);
#10972=ADVANCED_FACE('',(#3096),#2667,.F.);
#10973=ADVANCED_FACE('',(#3097),#2668,.F.);
#10974=ADVANCED_FACE('',(#3098),#2669,.F.);
#10975=ADVANCED_FACE('',(#3099),#2670,.F.);
#10976=ADVANCED_FACE('',(#3100),#2671,.F.);
#10977=ADVANCED_FACE('',(#3101),#706,.F.);
#10978=ADVANCED_FACE('',(#3102),#2672,.F.);
#10979=ADVANCED_FACE('',(#3103),#707,.F.);
#10980=ADVANCED_FACE('',(#3104),#2673,.F.);
#10981=ADVANCED_FACE('',(#3105),#708,.F.);
#10982=ADVANCED_FACE('',(#3106),#2674,.F.);
#10983=ADVANCED_FACE('',(#3107),#709,.F.);
#10984=ADVANCED_FACE('',(#3108),#2675,.F.);
#10985=ADVANCED_FACE('',(#3109),#2676,.F.);
#10986=ADVANCED_FACE('',(#3110),#2677,.F.);
#10987=ADVANCED_FACE('',(#3111),#2678,.F.);
#10988=ADVANCED_FACE('',(#3112),#2679,.F.);
#10989=ADVANCED_FACE('',(#3113),#2680,.F.);
#10990=ADVANCED_FACE('',(#3114),#710,.F.);
#10991=ADVANCED_FACE('',(#3115),#2681,.F.);
#10992=ADVANCED_FACE('',(#3116),#711,.F.);
#10993=ADVANCED_FACE('',(#3117),#2682,.F.);
#10994=ADVANCED_FACE('',(#3118),#712,.F.);
#10995=ADVANCED_FACE('',(#3119),#2683,.F.);
#10996=ADVANCED_FACE('',(#3120),#713,.F.);
#10997=ADVANCED_FACE('',(#3121),#2684,.F.);
#10998=ADVANCED_FACE('',(#3122),#2685,.F.);
#10999=ADVANCED_FACE('',(#3123),#2686,.F.);
#11000=ADVANCED_FACE('',(#3124),#2687,.F.);
#11001=ADVANCED_FACE('',(#3125),#2688,.F.);
#11002=ADVANCED_FACE('',(#3126),#2689,.F.);
#11003=ADVANCED_FACE('',(#3127),#714,.F.);
#11004=ADVANCED_FACE('',(#3128),#2690,.F.);
#11005=ADVANCED_FACE('',(#3129),#715,.F.);
#11006=ADVANCED_FACE('',(#3130),#2691,.F.);
#11007=ADVANCED_FACE('',(#3131),#716,.F.);
#11008=ADVANCED_FACE('',(#3132),#2692,.F.);
#11009=ADVANCED_FACE('',(#3133),#717,.F.);
#11010=ADVANCED_FACE('',(#3134),#2693,.F.);
#11011=ADVANCED_FACE('',(#3135),#2694,.F.);
#11012=ADVANCED_FACE('',(#3136),#2695,.F.);
#11013=ADVANCED_FACE('',(#3137),#718,.F.);
#11014=ADVANCED_FACE('',(#3138),#2696,.F.);
#11015=ADVANCED_FACE('',(#3139),#719,.F.);
#11016=ADVANCED_FACE('',(#3140),#2697,.F.);
#11017=ADVANCED_FACE('',(#3141),#720,.F.);
#11018=ADVANCED_FACE('',(#3142),#2698,.F.);
#11019=ADVANCED_FACE('',(#3143),#721,.F.);
#11020=ADVANCED_FACE('',(#3144),#2699,.F.);
#11021=ADVANCED_FACE('',(#3145),#2700,.F.);
#11022=ADVANCED_FACE('',(#3146),#2701,.F.);
#11023=ADVANCED_FACE('',(#3147),#2702,.F.);
#11024=ADVANCED_FACE('',(#3148),#2703,.F.);
#11025=ADVANCED_FACE('',(#3149,#187,#188,#189,#190,#191,#192,#193,#194,
#195,#196,#197,#198,#199,#200,#201,#202,#203,#204,#205,#206,#207,#208,#209,
#210,#211,#212,#213,#214,#215,#216,#217,#218,#219,#220,#221,#222,#223,#224,
#225,#226,#227,#228,#229,#230,#231,#232,#233,#234,#235,#236,#237,#238,#239,
#240,#241,#242,#243,#244,#245,#246,#247,#248,#249,#250,#251,#252,#253,#254,
#255,#256),#722,.T.);
#11026=ADVANCED_FACE('',(#3150),#2704,.F.);
#11027=ADVANCED_FACE('',(#3151,#257,#258,#259,#260,#261,#262,#263,#264,
#265,#266,#267,#268,#269,#270,#271,#272,#273,#274,#275,#276,#277,#278,#279,
#280,#281,#282,#283,#284,#285,#286,#287,#288,#289,#290,#291,#292,#293,#294,
#295,#296,#297,#298,#299,#300,#301,#302,#303),#723,.F.);
#11028=ADVANCED_FACE('',(#3152),#2705,.T.);
#11029=ADVANCED_FACE('',(#3153,#304,#305,#306,#307,#308,#309,#310,#311,
#312,#313,#314,#315,#316,#317,#318,#319,#320,#321,#322,#323,#324,#325,#326,
#327,#328,#329,#330,#331,#332,#333,#334,#335,#336,#337,#338,#339,#340,#341,
#342,#343,#344,#345,#346,#347,#348,#349,#350,#351,#352,#353,#354,#355,#356,
#357,#358,#359,#360,#361,#362,#363,#364,#365,#366,#367,#368,#369,#370,#371,
#372,#373),#724,.T.);
#11030=ADVANCED_FACE('',(#3154),#725,.T.);
#11031=ADVANCED_FACE('',(#3155),#2706,.T.);
#11032=ADVANCED_FACE('',(#3156),#2707,.F.);
#11033=ADVANCED_FACE('',(#3157),#2708,.F.);
#11034=ADVANCED_FACE('',(#3158),#2709,.F.);
#11035=ADVANCED_FACE('',(#3159),#2710,.F.);
#11036=ADVANCED_FACE('',(#3160),#2711,.F.);
#11037=ADVANCED_FACE('',(#3161),#2712,.F.);
#11038=ADVANCED_FACE('',(#3162),#2713,.F.);
#11039=ADVANCED_FACE('',(#3163),#2714,.F.);
#11040=ADVANCED_FACE('',(#3164),#2715,.F.);
#11041=ADVANCED_FACE('',(#3165),#2716,.F.);
#11042=ADVANCED_FACE('',(#3166),#2717,.F.);
#11043=ADVANCED_FACE('',(#3167),#2718,.F.);
#11044=ADVANCED_FACE('',(#3168),#2719,.F.);
#11045=ADVANCED_FACE('',(#3169),#2720,.F.);
#11046=ADVANCED_FACE('',(#3170),#2721,.F.);
#11047=ADVANCED_FACE('',(#3171),#2722,.F.);
#11048=ADVANCED_FACE('',(#3172),#2723,.F.);
#11049=ADVANCED_FACE('',(#3173),#2724,.F.);
#11050=ADVANCED_FACE('',(#3174),#2725,.F.);
#11051=ADVANCED_FACE('',(#3175),#2726,.F.);
#11052=ADVANCED_FACE('',(#3176),#2727,.F.);
#11053=ADVANCED_FACE('',(#3177),#2728,.F.);
#11054=ADVANCED_FACE('',(#3178),#2729,.F.);
#11055=ADVANCED_FACE('',(#3179),#2730,.F.);
#11056=ADVANCED_FACE('',(#3180),#2731,.F.);
#11057=ADVANCED_FACE('',(#3181),#2732,.F.);
#11058=ADVANCED_FACE('',(#3182),#2733,.F.);
#11059=ADVANCED_FACE('',(#3183),#2734,.F.);
#11060=ADVANCED_FACE('',(#3184),#2735,.F.);
#11061=ADVANCED_FACE('',(#3185),#2736,.F.);
#11062=ADVANCED_FACE('',(#3186),#2737,.F.);
#11063=ADVANCED_FACE('',(#3187),#2738,.F.);
#11064=ADVANCED_FACE('',(#3188),#2739,.F.);
#11065=ADVANCED_FACE('',(#3189),#2740,.F.);
#11066=ADVANCED_FACE('',(#3190),#2741,.F.);
#11067=ADVANCED_FACE('',(#3191),#2742,.F.);
#11068=ADVANCED_FACE('',(#3192),#2743,.F.);
#11069=ADVANCED_FACE('',(#3193),#2744,.F.);
#11070=ADVANCED_FACE('',(#3194),#2745,.F.);
#11071=ADVANCED_FACE('',(#3195),#2746,.F.);
#11072=ADVANCED_FACE('',(#3196),#2747,.F.);
#11073=ADVANCED_FACE('',(#3197),#2748,.F.);
#11074=ADVANCED_FACE('',(#3198),#2749,.F.);
#11075=ADVANCED_FACE('',(#3199),#2750,.F.);
#11076=ADVANCED_FACE('',(#3200),#2751,.F.);
#11077=ADVANCED_FACE('',(#3201),#2752,.F.);
#11078=ADVANCED_FACE('',(#3202),#2753,.F.);
#11079=ADVANCED_FACE('',(#3203),#726,.T.);
#11080=ADVANCED_FACE('',(#3204,#374,#375,#376,#377,#378,#379,#380,#381,
#382,#383,#384,#385,#386,#387,#388,#389,#390,#391,#392,#393,#394,#395,#396,
#397,#398,#399,#400,#401,#402,#403,#404,#405,#406,#407,#408,#409,#410,#411,
#412,#413,#414,#415,#416,#417,#418,#419,#420),#727,.T.);
#11081=ADVANCED_FACE('',(#3205),#2754,.F.);
#11082=ADVANCED_FACE('',(#3206),#2755,.F.);
#11083=ADVANCED_FACE('',(#3207),#2756,.F.);
#11084=ADVANCED_FACE('',(#3208),#2757,.F.);
#11085=ADVANCED_FACE('',(#3209),#2758,.F.);
#11086=ADVANCED_FACE('',(#3210),#2759,.F.);
#11087=ADVANCED_FACE('',(#3211),#2760,.F.);
#11088=ADVANCED_FACE('',(#3212),#2761,.F.);
#11089=ADVANCED_FACE('',(#3213),#2762,.F.);
#11090=ADVANCED_FACE('',(#3214),#2763,.F.);
#11091=ADVANCED_FACE('',(#3215),#2764,.F.);
#11092=ADVANCED_FACE('',(#3216),#2765,.F.);
#11093=ADVANCED_FACE('',(#3217),#2766,.F.);
#11094=ADVANCED_FACE('',(#3218),#2767,.F.);
#11095=ADVANCED_FACE('',(#3219),#2768,.F.);
#11096=ADVANCED_FACE('',(#3220),#2769,.F.);
#11097=ADVANCED_FACE('',(#3221),#2770,.F.);
#11098=ADVANCED_FACE('',(#3222),#2771,.F.);
#11099=ADVANCED_FACE('',(#3223),#2772,.F.);
#11100=ADVANCED_FACE('',(#3224),#2773,.F.);
#11101=ADVANCED_FACE('',(#3225),#2774,.F.);
#11102=ADVANCED_FACE('',(#3226),#2775,.F.);
#11103=ADVANCED_FACE('',(#3227),#2776,.F.);
#11104=ADVANCED_FACE('',(#3228),#2777,.F.);
#11105=ADVANCED_FACE('',(#3229),#2778,.F.);
#11106=ADVANCED_FACE('',(#3230),#2779,.F.);
#11107=ADVANCED_FACE('',(#3231),#2780,.F.);
#11108=ADVANCED_FACE('',(#3232),#2781,.F.);
#11109=ADVANCED_FACE('',(#3233),#2782,.F.);
#11110=ADVANCED_FACE('',(#3234),#2783,.F.);
#11111=ADVANCED_FACE('',(#3235),#2784,.F.);
#11112=ADVANCED_FACE('',(#3236),#2785,.F.);
#11113=ADVANCED_FACE('',(#3237),#2786,.F.);
#11114=ADVANCED_FACE('',(#3238),#2787,.F.);
#11115=ADVANCED_FACE('',(#3239),#2788,.F.);
#11116=ADVANCED_FACE('',(#3240),#2789,.F.);
#11117=ADVANCED_FACE('',(#3241),#2790,.F.);
#11118=ADVANCED_FACE('',(#3242),#2791,.F.);
#11119=ADVANCED_FACE('',(#3243),#2792,.F.);
#11120=ADVANCED_FACE('',(#3244),#2793,.F.);
#11121=ADVANCED_FACE('',(#3245),#2794,.F.);
#11122=ADVANCED_FACE('',(#3246),#2795,.F.);
#11123=ADVANCED_FACE('',(#3247),#2796,.F.);
#11124=ADVANCED_FACE('',(#3248),#2797,.F.);
#11125=ADVANCED_FACE('',(#3249),#2798,.F.);
#11126=ADVANCED_FACE('',(#3250),#2799,.F.);
#11127=ADVANCED_FACE('',(#3251),#2800,.F.);
#11128=ADVANCED_FACE('',(#3252),#728,.T.);
#11129=ADVANCED_FACE('',(#3253),#729,.T.);
#11130=ADVANCED_FACE('',(#3254,#421,#422,#423,#424,#425,#426,#427,#428,
#429,#430,#431,#432,#433,#434,#435,#436,#437,#438,#439,#440,#441,#442,#443,
#444,#445,#446,#447,#448,#449,#450,#451,#452,#453,#454,#455,#456,#457,#458,
#459,#460,#461,#462,#463,#464,#465,#466,#467),#730,.T.);
#11131=ADVANCED_FACE('',(#3255,#468,#469,#470,#471,#472,#473,#474,#475,
#476,#477,#478,#479,#480,#481,#482,#483,#484,#485,#486,#487,#488,#489,#490,
#491,#492,#493,#494,#495,#496,#497,#498,#499,#500,#501,#502,#503,#504,#505,
#506,#507,#508,#509,#510,#511,#512,#513,#514),#731,.F.);
#11132=ADVANCED_FACE('',(#3256),#2801,.F.);
#11133=ADVANCED_FACE('',(#3257),#2802,.F.);
#11134=ADVANCED_FACE('',(#3258),#2803,.F.);
#11135=ADVANCED_FACE('',(#3259),#2804,.F.);
#11136=ADVANCED_FACE('',(#3260,#515,#516,#517,#518,#519,#520,#521,#522,
#523,#524,#525),#732,.F.);
#11137=ADVANCED_FACE('',(#3261),#2805,.T.);
#11138=ADVANCED_FACE('',(#3262,#526,#527,#528,#529,#530,#531,#532,#533,
#534,#535,#536),#733,.T.);
#11139=ADVANCED_FACE('',(#3263),#2806,.F.);
#11140=ADVANCED_FACE('',(#3264),#2807,.F.);
#11141=ADVANCED_FACE('',(#3265),#2808,.F.);
#11142=ADVANCED_FACE('',(#3266),#2809,.F.);
#11143=ADVANCED_FACE('',(#3267),#2810,.F.);
#11144=ADVANCED_FACE('',(#3268),#2811,.F.);
#11145=ADVANCED_FACE('',(#3269),#2812,.F.);
#11146=ADVANCED_FACE('',(#3270),#2813,.F.);
#11147=ADVANCED_FACE('',(#3271),#2814,.F.);
#11148=ADVANCED_FACE('',(#3272),#2815,.F.);
#11149=ADVANCED_FACE('',(#3273),#2816,.F.);
#11150=ADVANCED_FACE('',(#3274),#734,.T.);
#11151=ADVANCED_FACE('',(#3275),#735,.T.);
#11152=ADVANCED_FACE('',(#3276),#736,.T.);
#11153=ADVANCED_FACE('',(#3277),#737,.T.);
#11154=ADVANCED_FACE('',(#3278),#738,.T.);
#11155=ADVANCED_FACE('',(#3279,#537,#538,#539,#540,#541,#542,#543,#544,
#545,#546,#547),#739,.F.);
#11156=ADVANCED_FACE('',(#3280),#2817,.F.);
#11157=ADVANCED_FACE('',(#3281),#2818,.F.);
#11158=ADVANCED_FACE('',(#3282),#2819,.F.);
#11159=ADVANCED_FACE('',(#3283),#2820,.F.);
#11160=ADVANCED_FACE('',(#3284),#2821,.F.);
#11161=ADVANCED_FACE('',(#3285),#2822,.F.);
#11162=ADVANCED_FACE('',(#3286),#2823,.F.);
#11163=ADVANCED_FACE('',(#3287),#2824,.F.);
#11164=ADVANCED_FACE('',(#3288),#2825,.F.);
#11165=ADVANCED_FACE('',(#3289),#2826,.F.);
#11166=ADVANCED_FACE('',(#3290),#2827,.F.);
#11167=ADVANCED_FACE('',(#3291),#740,.T.);
#11168=ADVANCED_FACE('',(#3292),#741,.T.);
#11169=ADVANCED_FACE('',(#3293),#742,.T.);
#11170=ADVANCED_FACE('',(#3294),#743,.T.);
#11171=ADVANCED_FACE('',(#3295),#744,.T.);
#11172=ADVANCED_FACE('',(#3296,#548,#549,#550,#551,#552,#553,#554,#555,
#556,#557,#558),#745,.T.);
#11173=ADVANCED_FACE('',(#3297,#559,#560,#561),#746,.T.);
#11174=ADVANCED_FACE('',(#3298,#562),#747,.T.);
#11175=ADVANCED_FACE('',(#3299),#748,.T.);
#11176=ADVANCED_FACE('',(#3300,#563,#564),#749,.T.);
#11177=ADVANCED_FACE('',(#3301),#750,.T.);
#11178=ADVANCED_FACE('',(#3302),#751,.T.);
#11179=ADVANCED_FACE('',(#3303),#2828,.F.);
#11180=ADVANCED_FACE('',(#3304),#752,.T.);
#11181=ADVANCED_FACE('',(#3305),#753,.T.);
#11182=ADVANCED_FACE('',(#3306),#754,.T.);
#11183=ADVANCED_FACE('',(#3307),#755,.T.);
#11184=ADVANCED_FACE('',(#3308),#756,.T.);
#11185=ADVANCED_FACE('',(#3309),#757,.T.);
#11186=ADVANCED_FACE('',(#3310,#565),#758,.T.);
#11187=ADVANCED_FACE('',(#3311,#566),#759,.F.);
#11188=ADVANCED_FACE('',(#3312),#2829,.F.);
#11189=ADVANCED_FACE('',(#3313),#2830,.F.);
#11190=ADVANCED_FACE('',(#3314),#2831,.F.);
#11191=ADVANCED_FACE('',(#3315),#2832,.F.);
#11192=ADVANCED_FACE('',(#3316,#567,#568,#569,#570,#571,#572,#573,#574,
#575,#576,#577),#760,.F.);
#11193=ADVANCED_FACE('',(#3317),#2833,.T.);
#11194=ADVANCED_FACE('',(#3318,#578,#579,#580,#581,#582,#583,#584,#585,
#586,#587,#588),#761,.T.);
#11195=ADVANCED_FACE('',(#3319),#2834,.F.);
#11196=ADVANCED_FACE('',(#3320),#2835,.F.);
#11197=ADVANCED_FACE('',(#3321),#2836,.F.);
#11198=ADVANCED_FACE('',(#3322),#2837,.F.);
#11199=ADVANCED_FACE('',(#3323),#2838,.F.);
#11200=ADVANCED_FACE('',(#3324),#2839,.F.);
#11201=ADVANCED_FACE('',(#3325),#2840,.F.);
#11202=ADVANCED_FACE('',(#3326),#2841,.F.);
#11203=ADVANCED_FACE('',(#3327),#2842,.F.);
#11204=ADVANCED_FACE('',(#3328),#2843,.F.);
#11205=ADVANCED_FACE('',(#3329),#2844,.F.);
#11206=ADVANCED_FACE('',(#3330),#762,.T.);
#11207=ADVANCED_FACE('',(#3331),#763,.T.);
#11208=ADVANCED_FACE('',(#3332),#764,.T.);
#11209=ADVANCED_FACE('',(#3333),#765,.T.);
#11210=ADVANCED_FACE('',(#3334),#766,.T.);
#11211=ADVANCED_FACE('',(#3335,#589,#590,#591,#592,#593,#594,#595,#596,
#597,#598,#599),#767,.F.);
#11212=ADVANCED_FACE('',(#3336),#2845,.F.);
#11213=ADVANCED_FACE('',(#3337),#2846,.F.);
#11214=ADVANCED_FACE('',(#3338),#2847,.F.);
#11215=ADVANCED_FACE('',(#3339),#2848,.F.);
#11216=ADVANCED_FACE('',(#3340),#2849,.F.);
#11217=ADVANCED_FACE('',(#3341),#2850,.F.);
#11218=ADVANCED_FACE('',(#3342),#2851,.F.);
#11219=ADVANCED_FACE('',(#3343),#2852,.F.);
#11220=ADVANCED_FACE('',(#3344),#2853,.F.);
#11221=ADVANCED_FACE('',(#3345),#2854,.F.);
#11222=ADVANCED_FACE('',(#3346),#2855,.F.);
#11223=ADVANCED_FACE('',(#3347),#768,.T.);
#11224=ADVANCED_FACE('',(#3348),#769,.T.);
#11225=ADVANCED_FACE('',(#3349),#770,.T.);
#11226=ADVANCED_FACE('',(#3350),#771,.T.);
#11227=ADVANCED_FACE('',(#3351),#772,.T.);
#11228=ADVANCED_FACE('',(#3352,#600,#601,#602,#603,#604,#605,#606,#607,
#608,#609,#610),#773,.T.);
#11229=ADVANCED_FACE('',(#3353,#611,#612,#613),#774,.T.);
#11230=ADVANCED_FACE('',(#3354,#614),#775,.T.);
#11231=ADVANCED_FACE('',(#3355),#776,.T.);
#11232=ADVANCED_FACE('',(#3356,#615,#616),#777,.T.);
#11233=ADVANCED_FACE('',(#3357),#778,.T.);
#11234=ADVANCED_FACE('',(#3358),#779,.T.);
#11235=ADVANCED_FACE('',(#3359,#617),#780,.F.);
#11236=ADVANCED_FACE('',(#3360),#781,.T.);
#11237=ADVANCED_FACE('',(#3361),#782,.T.);
#11238=ADVANCED_FACE('',(#3362),#783,.T.);
#11239=ADVANCED_FACE('',(#3363),#784,.T.);
#11240=ADVANCED_FACE('',(#3364),#785,.T.);
#11241=ADVANCED_FACE('',(#3365),#786,.T.);
#11242=ADVANCED_FACE('',(#3366),#787,.T.);
#11243=ADVANCED_FACE('',(#3367),#2856,.T.);
#11244=ADVANCED_FACE('',(#3368),#788,.F.);
#11245=ADVANCED_FACE('',(#3369),#2857,.F.);
#11246=ADVANCED_FACE('',(#3370),#789,.T.);
#11247=ADVANCED_FACE('',(#3371),#790,.T.);
#11248=ADVANCED_FACE('',(#3372),#791,.T.);
#11249=ADVANCED_FACE('',(#3373),#792,.T.);
#11250=ADVANCED_FACE('',(#3374),#793,.T.);
#11251=ADVANCED_FACE('',(#3375),#794,.T.);
#11252=ADVANCED_FACE('',(#3376,#618),#795,.T.);
#11253=ADVANCED_FACE('',(#3377,#619),#796,.F.);
#11254=ADVANCED_FACE('',(#3378),#2858,.F.);
#11255=ADVANCED_FACE('',(#3379),#797,.T.);
#11256=ADVANCED_FACE('',(#3380),#798,.T.);
#11257=ADVANCED_FACE('',(#3381),#799,.T.);
#11258=ADVANCED_FACE('',(#3382),#800,.T.);
#11259=ADVANCED_FACE('',(#3383),#801,.T.);
#11260=ADVANCED_FACE('',(#3384),#802,.T.);
#11261=ADVANCED_FACE('',(#3385,#620),#803,.T.);
#11262=ADVANCED_FACE('',(#3386,#621),#804,.F.);
#11263=ADVANCED_FACE('',(#3387),#805,.F.);
#11264=ADVANCED_FACE('',(#3388),#2859,.F.);
#11265=ADVANCED_FACE('',(#3389),#806,.F.);
#11266=ADVANCED_FACE('',(#3390),#807,.F.);
#11267=ADVANCED_FACE('',(#3391),#2860,.T.);
#11268=ADVANCED_FACE('',(#3392),#808,.F.);
#11269=ADVANCED_FACE('',(#3393),#2861,.F.);
#11270=ADVANCED_FACE('',(#3394),#2862,.T.);
#11271=ADVANCED_FACE('',(#3395),#809,.T.);
#11272=ADVANCED_FACE('',(#3396),#810,.T.);
#11273=ADVANCED_FACE('',(#3397),#2863,.F.);
#11274=ADVANCED_FACE('',(#3398),#811,.T.);
#11275=ADVANCED_FACE('',(#3399),#812,.T.);
#11276=ADVANCED_FACE('',(#3400),#2864,.T.);
#11277=ADVANCED_FACE('',(#3401),#813,.T.);
#11278=ADVANCED_FACE('',(#3402),#2865,.F.);
#11279=ADVANCED_FACE('',(#3403),#814,.T.);
#11280=ADVANCED_FACE('',(#3404),#2866,.T.);
#11281=ADVANCED_FACE('',(#3405),#815,.T.);
#11282=ADVANCED_FACE('',(#3406),#816,.T.);
#11283=ADVANCED_FACE('',(#3407),#817,.T.);
#11284=ADVANCED_FACE('',(#3408),#2867,.F.);
#11285=ADVANCED_FACE('',(#3409),#818,.F.);
#11286=ADVANCED_FACE('',(#3410),#2868,.F.);
#11287=ADVANCED_FACE('',(#3411),#819,.F.);
#11288=ADVANCED_FACE('',(#3412),#820,.F.);
#11289=ADVANCED_FACE('',(#3413),#821,.F.);
#11290=ADVANCED_FACE('',(#3414),#2869,.T.);
#11291=ADVANCED_FACE('',(#3415),#822,.F.);
#11292=ADVANCED_FACE('',(#3416),#2870,.T.);
#11293=ADVANCED_FACE('',(#3417),#823,.T.);
#11294=ADVANCED_FACE('',(#3418),#2871,.F.);
#11295=ADVANCED_FACE('',(#3419),#824,.T.);
#11296=ADVANCED_FACE('',(#3420),#2872,.F.);
#11297=ADVANCED_FACE('',(#3421),#825,.T.);
#11298=ADVANCED_FACE('',(#3422),#826,.T.);
#11299=ADVANCED_FACE('',(#3423),#827,.T.);
#11300=ADVANCED_FACE('',(#3424),#2873,.T.);
#11301=ADVANCED_FACE('',(#3425),#828,.T.);
#11302=ADVANCED_FACE('',(#3426),#2874,.T.);
#11303=ADVANCED_FACE('',(#3427,#622),#829,.T.);
#11304=ADVANCED_FACE('',(#3428,#623),#830,.F.);
#11305=ADVANCED_FACE('',(#3429),#2875,.F.);
#11306=ADVANCED_FACE('',(#3430),#831,.T.);
#11307=ADVANCED_FACE('',(#3431),#832,.T.);
#11308=ADVANCED_FACE('',(#3432),#833,.T.);
#11309=ADVANCED_FACE('',(#3433),#834,.T.);
#11310=ADVANCED_FACE('',(#3434),#835,.T.);
#11311=ADVANCED_FACE('',(#3435),#836,.T.);
#11312=ADVANCED_FACE('',(#3436,#624),#837,.T.);
#11313=ADVANCED_FACE('',(#3437,#625),#838,.F.);
#11314=CLOSED_SHELL('',(#10768,#10769,#10770,#10771,#10772,#10773,#10774,
#10775,#10776,#10777,#10778,#10779,#10780));
#11315=CLOSED_SHELL('',(#10781,#10782,#10783,#10784,#10785,#10786,#10787,
#10788,#10789,#10790,#10791,#10792,#10793,#10794,#10795,#10796));
#11316=CLOSED_SHELL('',(#10797,#10798,#10799,#10800,#10801,#10802,#10803,
#10804,#10805,#10806,#10807,#10808,#10809,#10810,#10811,#10812,#10813,#10814,
#10815,#10816,#10817,#10818,#10819,#10820,#10821,#10822,#10823,#10824,#10825,
#10826,#10827,#10828,#10829,#10830,#10831,#10832,#10833,#10834,#10835,#10836,
#10837,#10838,#10839,#10840,#10841));
#11317=CLOSED_SHELL('',(#10842,#10843,#10844,#10845,#10846,#10847,#10848,
#10849,#10850,#10851));
#11318=CLOSED_SHELL('',(#10852,#10853,#10854,#10855,#10856,#10857,#10858,
#10859,#10860,#10861,#10862,#10863,#10864,#10865,#10866,#10867,#10868,#10869,
#10870,#10871,#10872,#10873,#10874,#10875,#10876,#10877,#10878,#10879,#10880,
#10881,#10882,#10883,#10884,#10885,#10886,#10887,#10888,#10889,#10890,#10891,
#10892,#10893));
#11319=CLOSED_SHELL('',(#10894,#10895,#10896,#10897,#10898,#10899,#10900,
#10901,#10902,#10903,#10904,#10905,#10906,#10907,#10908,#10909,#10910,#10911,
#10912,#10913,#10914,#10915,#10916,#10917,#10918,#10919,#10920,#10921,#10922,
#10923,#10924,#10925,#10926,#10927,#10928,#10929,#10930,#10931,#10932,#10933,
#10934,#10935,#10936,#10937,#10938,#10939,#10940,#10941,#10942,#10943,#10944,
#10945,#10946,#10947,#10948,#10949,#10950,#10951,#10952,#10953,#10954,#10955,
#10956,#10957,#10958,#10959,#10960,#10961,#10962,#10963,#10964,#10965,#10966,
#10967,#10968,#10969,#10970,#10971,#10972,#10973,#10974,#10975,#10976,#10977,
#10978,#10979,#10980,#10981,#10982,#10983,#10984,#10985,#10986,#10987,#10988,
#10989,#10990,#10991,#10992,#10993,#10994,#10995,#10996,#10997,#10998,#10999,
#11000,#11001,#11002,#11003,#11004,#11005,#11006,#11007,#11008,#11009,#11010,
#11011,#11012,#11013,#11014,#11015,#11016,#11017,#11018,#11019,#11020,#11021,
#11022,#11023,#11024,#11025,#11026,#11027,#11028,#11029,#11030,#11031,#11032,
#11033,#11034,#11035,#11036,#11037,#11038,#11039,#11040,#11041,#11042,#11043,
#11044,#11045,#11046,#11047,#11048,#11049,#11050,#11051,#11052,#11053,#11054,
#11055,#11056,#11057,#11058,#11059,#11060,#11061,#11062,#11063,#11064,#11065,
#11066,#11067,#11068,#11069,#11070,#11071,#11072,#11073,#11074,#11075,#11076,
#11077,#11078,#11079,#11080,#11081,#11082,#11083,#11084,#11085,#11086,#11087,
#11088,#11089,#11090,#11091,#11092,#11093,#11094,#11095,#11096,#11097,#11098,
#11099,#11100,#11101,#11102,#11103,#11104,#11105,#11106,#11107,#11108,#11109,
#11110,#11111,#11112,#11113,#11114,#11115,#11116,#11117,#11118,#11119,#11120,
#11121,#11122,#11123,#11124,#11125,#11126,#11127,#11128,#11129,#11130,#11131));
#11320=CLOSED_SHELL('',(#11132,#11133,#11134,#11135,#11136,#11137,#11138,
#11139,#11140,#11141,#11142,#11143,#11144,#11145,#11146,#11147,#11148,#11149,
#11150,#11151,#11152,#11153,#11154,#11155,#11156,#11157,#11158,#11159,#11160,
#11161,#11162,#11163,#11164,#11165,#11166,#11167,#11168,#11169,#11170,#11171,
#11172,#11173,#11174,#11175,#11176,#11177,#11178));
#11321=CLOSED_SHELL('',(#11179,#11180,#11181,#11182,#11183,#11184,#11185,
#11186,#11187));
#11322=CLOSED_SHELL('',(#11188,#11189,#11190,#11191,#11192,#11193,#11194,
#11195,#11196,#11197,#11198,#11199,#11200,#11201,#11202,#11203,#11204,#11205,
#11206,#11207,#11208,#11209,#11210,#11211,#11212,#11213,#11214,#11215,#11216,
#11217,#11218,#11219,#11220,#11221,#11222,#11223,#11224,#11225,#11226,#11227,
#11228,#11229,#11230,#11231,#11232,#11233,#11234));
#11323=CLOSED_SHELL('',(#11235,#11236,#11237,#11238,#11239,#11240,#11241,
#11242,#11243,#11244));
#11324=CLOSED_SHELL('',(#11245,#11246,#11247,#11248,#11249,#11250,#11251,
#11252,#11253));
#11325=CLOSED_SHELL('',(#11254,#11255,#11256,#11257,#11258,#11259,#11260,
#11261,#11262));
#11326=CLOSED_SHELL('',(#11263,#11264,#11265,#11266,#11267,#11268,#11269,
#11270,#11271,#11272,#11273,#11274,#11275,#11276,#11277,#11278,#11279,#11280,
#11281,#11282,#11283,#11284,#11285,#11286,#11287,#11288,#11289,#11290,#11291,
#11292,#11293,#11294,#11295,#11296,#11297,#11298,#11299,#11300,#11301,#11302,
#11303,#11304));
#11327=CLOSED_SHELL('',(#11305,#11306,#11307,#11308,#11309,#11310,#11311,
#11312,#11313));
#11328=DERIVED_UNIT_ELEMENT(#11356,1.);
#11329=DERIVED_UNIT_ELEMENT(#19222,-3.);
#11330=DERIVED_UNIT_ELEMENT(#11356,1.);
#11331=DERIVED_UNIT_ELEMENT(#19222,-3.);
#11332=DERIVED_UNIT_ELEMENT(#11356,1.);
#11333=DERIVED_UNIT_ELEMENT(#19222,-3.);
#11334=DERIVED_UNIT_ELEMENT(#11356,1.);
#11335=DERIVED_UNIT_ELEMENT(#19222,-3.);
#11336=DERIVED_UNIT_ELEMENT(#11356,1.);
#11337=DERIVED_UNIT_ELEMENT(#19222,-3.);
#11338=DERIVED_UNIT_ELEMENT(#11356,1.);
#11339=DERIVED_UNIT_ELEMENT(#19222,-3.);
#11340=DERIVED_UNIT_ELEMENT(#11356,1.);
#11341=DERIVED_UNIT_ELEMENT(#19222,-3.);
#11342=DERIVED_UNIT_ELEMENT(#11356,1.);
#11343=DERIVED_UNIT_ELEMENT(#19222,-3.);
#11344=DERIVED_UNIT_ELEMENT(#11356,1.);
#11345=DERIVED_UNIT_ELEMENT(#19222,-3.);
#11346=DERIVED_UNIT_ELEMENT(#11356,1.);
#11347=DERIVED_UNIT_ELEMENT(#19222,-3.);
#11348=DERIVED_UNIT_ELEMENT(#11356,1.);
#11349=DERIVED_UNIT_ELEMENT(#19222,-3.);
#11350=DERIVED_UNIT_ELEMENT(#11356,1.);
#11351=DERIVED_UNIT_ELEMENT(#19222,-3.);
#11352=DERIVED_UNIT_ELEMENT(#11356,1.);
#11353=DERIVED_UNIT_ELEMENT(#19222,-3.);
#11354=DERIVED_UNIT_ELEMENT(#11356,1.);
#11355=DERIVED_UNIT_ELEMENT(#19222,-3.);
#11356=(
MASS_UNIT()
NAMED_UNIT(*)
SI_UNIT(.KILO.,.GRAM.)
);
#11357=DERIVED_UNIT((#11328,#11329));
#11358=DERIVED_UNIT((#11330,#11331));
#11359=DERIVED_UNIT((#11332,#11333));
#11360=DERIVED_UNIT((#11334,#11335));
#11361=DERIVED_UNIT((#11336,#11337));
#11362=DERIVED_UNIT((#11338,#11339));
#11363=DERIVED_UNIT((#11340,#11341));
#11364=DERIVED_UNIT((#11342,#11343));
#11365=DERIVED_UNIT((#11344,#11345));
#11366=DERIVED_UNIT((#11346,#11347));
#11367=DERIVED_UNIT((#11348,#11349));
#11368=DERIVED_UNIT((#11350,#11351));
#11369=DERIVED_UNIT((#11352,#11353));
#11370=DERIVED_UNIT((#11354,#11355));
#11371=MEASURE_REPRESENTATION_ITEM('density measure',
POSITIVE_RATIO_MEASURE(7850.),#11357);
#11372=MEASURE_REPRESENTATION_ITEM('density measure',
POSITIVE_RATIO_MEASURE(7850.),#11358);
#11373=MEASURE_REPRESENTATION_ITEM('density measure',
POSITIVE_RATIO_MEASURE(7850.),#11359);
#11374=MEASURE_REPRESENTATION_ITEM('density measure',
POSITIVE_RATIO_MEASURE(7850.),#11360);
#11375=MEASURE_REPRESENTATION_ITEM('density measure',
POSITIVE_RATIO_MEASURE(7850.),#11361);
#11376=MEASURE_REPRESENTATION_ITEM('density measure',
POSITIVE_RATIO_MEASURE(7850.),#11362);
#11377=MEASURE_REPRESENTATION_ITEM('density measure',
POSITIVE_RATIO_MEASURE(7850.),#11363);
#11378=MEASURE_REPRESENTATION_ITEM('density measure',
POSITIVE_RATIO_MEASURE(7850.),#11364);
#11379=MEASURE_REPRESENTATION_ITEM('density measure',
POSITIVE_RATIO_MEASURE(7850.),#11365);
#11380=MEASURE_REPRESENTATION_ITEM('density measure',
POSITIVE_RATIO_MEASURE(7850.),#11366);
#11381=MEASURE_REPRESENTATION_ITEM('density measure',
POSITIVE_RATIO_MEASURE(7850.),#11367);
#11382=MEASURE_REPRESENTATION_ITEM('density measure',
POSITIVE_RATIO_MEASURE(7850.),#11368);
#11383=MEASURE_REPRESENTATION_ITEM('density measure',
POSITIVE_RATIO_MEASURE(7850.),#11369);
#11384=MEASURE_REPRESENTATION_ITEM('density measure',
POSITIVE_RATIO_MEASURE(7850.),#11370);
#11385=PROPERTY_DEFINITION_REPRESENTATION(#11455,#11413);
#11386=PROPERTY_DEFINITION_REPRESENTATION(#11456,#11414);
#11387=PROPERTY_DEFINITION_REPRESENTATION(#11457,#11415);
#11388=PROPERTY_DEFINITION_REPRESENTATION(#11458,#11416);
#11389=PROPERTY_DEFINITION_REPRESENTATION(#11459,#11417);
#11390=PROPERTY_DEFINITION_REPRESENTATION(#11460,#11418);
#11391=PROPERTY_DEFINITION_REPRESENTATION(#11461,#11419);
#11392=PROPERTY_DEFINITION_REPRESENTATION(#11462,#11420);
#11393=PROPERTY_DEFINITION_REPRESENTATION(#11463,#11421);
#11394=PROPERTY_DEFINITION_REPRESENTATION(#11464,#11422);
#11395=PROPERTY_DEFINITION_REPRESENTATION(#11465,#11423);
#11396=PROPERTY_DEFINITION_REPRESENTATION(#11466,#11424);
#11397=PROPERTY_DEFINITION_REPRESENTATION(#11467,#11425);
#11398=PROPERTY_DEFINITION_REPRESENTATION(#11468,#11426);
#11399=PROPERTY_DEFINITION_REPRESENTATION(#11469,#11427);
#11400=PROPERTY_DEFINITION_REPRESENTATION(#11470,#11428);
#11401=PROPERTY_DEFINITION_REPRESENTATION(#11471,#11429);
#11402=PROPERTY_DEFINITION_REPRESENTATION(#11472,#11430);
#11403=PROPERTY_DEFINITION_REPRESENTATION(#11473,#11431);
#11404=PROPERTY_DEFINITION_REPRESENTATION(#11474,#11432);
#11405=PROPERTY_DEFINITION_REPRESENTATION(#11475,#11433);
#11406=PROPERTY_DEFINITION_REPRESENTATION(#11476,#11434);
#11407=PROPERTY_DEFINITION_REPRESENTATION(#11477,#11435);
#11408=PROPERTY_DEFINITION_REPRESENTATION(#11478,#11436);
#11409=PROPERTY_DEFINITION_REPRESENTATION(#11479,#11437);
#11410=PROPERTY_DEFINITION_REPRESENTATION(#11480,#11438);
#11411=PROPERTY_DEFINITION_REPRESENTATION(#11481,#11439);
#11412=PROPERTY_DEFINITION_REPRESENTATION(#11482,#11440);
#11413=REPRESENTATION('material name',(#11441),#19206);
#11414=REPRESENTATION('density',(#11371),#19206);
#11415=REPRESENTATION('material name',(#11442),#19207);
#11416=REPRESENTATION('density',(#11372),#19207);
#11417=REPRESENTATION('material name',(#11443),#19208);
#11418=REPRESENTATION('density',(#11373),#19208);
#11419=REPRESENTATION('material name',(#11444),#19209);
#11420=REPRESENTATION('density',(#11374),#19209);
#11421=REPRESENTATION('material name',(#11445),#19210);
#11422=REPRESENTATION('density',(#11375),#19210);
#11423=REPRESENTATION('material name',(#11446),#19211);
#11424=REPRESENTATION('density',(#11376),#19211);
#11425=REPRESENTATION('material name',(#11447),#19212);
#11426=REPRESENTATION('density',(#11377),#19212);
#11427=REPRESENTATION('material name',(#11448),#19213);
#11428=REPRESENTATION('density',(#11378),#19213);
#11429=REPRESENTATION('material name',(#11449),#19214);
#11430=REPRESENTATION('density',(#11379),#19214);
#11431=REPRESENTATION('material name',(#11450),#19215);
#11432=REPRESENTATION('density',(#11380),#19215);
#11433=REPRESENTATION('material name',(#11451),#19216);
#11434=REPRESENTATION('density',(#11381),#19216);
#11435=REPRESENTATION('material name',(#11452),#19217);
#11436=REPRESENTATION('density',(#11382),#19217);
#11437=REPRESENTATION('material name',(#11453),#19218);
#11438=REPRESENTATION('density',(#11383),#19218);
#11439=REPRESENTATION('material name',(#11454),#19219);
#11440=REPRESENTATION('density',(#11384),#19219);
#11441=DESCRIPTIVE_REPRESENTATION_ITEM('Steel','Steel');
#11442=DESCRIPTIVE_REPRESENTATION_ITEM('Steel','Steel');
#11443=DESCRIPTIVE_REPRESENTATION_ITEM('Steel','Steel');
#11444=DESCRIPTIVE_REPRESENTATION_ITEM('Steel','Steel');
#11445=DESCRIPTIVE_REPRESENTATION_ITEM('Steel','Steel');
#11446=DESCRIPTIVE_REPRESENTATION_ITEM('Steel','Steel');
#11447=DESCRIPTIVE_REPRESENTATION_ITEM('Steel','Steel');
#11448=DESCRIPTIVE_REPRESENTATION_ITEM('Steel','Steel');
#11449=DESCRIPTIVE_REPRESENTATION_ITEM('Steel','Steel');
#11450=DESCRIPTIVE_REPRESENTATION_ITEM('Steel','Steel');
#11451=DESCRIPTIVE_REPRESENTATION_ITEM('Steel','Steel');
#11452=DESCRIPTIVE_REPRESENTATION_ITEM('Steel','Steel');
#11453=DESCRIPTIVE_REPRESENTATION_ITEM('Steel','Steel');
#11454=DESCRIPTIVE_REPRESENTATION_ITEM('Steel','Steel');
#11455=PROPERTY_DEFINITION('material property','material name',#19286);
#11456=PROPERTY_DEFINITION('material property','density of part',#19286);
#11457=PROPERTY_DEFINITION('material property','material name',#19287);
#11458=PROPERTY_DEFINITION('material property','density of part',#19287);
#11459=PROPERTY_DEFINITION('material property','material name',#19288);
#11460=PROPERTY_DEFINITION('material property','density of part',#19288);
#11461=PROPERTY_DEFINITION('material property','material name',#19289);
#11462=PROPERTY_DEFINITION('material property','density of part',#19289);
#11463=PROPERTY_DEFINITION('material property','material name',#19290);
#11464=PROPERTY_DEFINITION('material property','density of part',#19290);
#11465=PROPERTY_DEFINITION('material property','material name',#19291);
#11466=PROPERTY_DEFINITION('material property','density of part',#19291);
#11467=PROPERTY_DEFINITION('material property','material name',#19292);
#11468=PROPERTY_DEFINITION('material property','density of part',#19292);
#11469=PROPERTY_DEFINITION('material property','material name',#19293);
#11470=PROPERTY_DEFINITION('material property','density of part',#19293);
#11471=PROPERTY_DEFINITION('material property','material name',#19294);
#11472=PROPERTY_DEFINITION('material property','density of part',#19294);
#11473=PROPERTY_DEFINITION('material property','material name',#19295);
#11474=PROPERTY_DEFINITION('material property','density of part',#19295);
#11475=PROPERTY_DEFINITION('material property','material name',#19296);
#11476=PROPERTY_DEFINITION('material property','density of part',#19296);
#11477=PROPERTY_DEFINITION('material property','material name',#19297);
#11478=PROPERTY_DEFINITION('material property','density of part',#19297);
#11479=PROPERTY_DEFINITION('material property','material name',#19298);
#11480=PROPERTY_DEFINITION('material property','density of part',#19298);
#11481=PROPERTY_DEFINITION('material property','material name',#19299);
#11482=PROPERTY_DEFINITION('material property','density of part',#19299);
#11483=AXIS2_PLACEMENT_3D('',#16073,#12728,#12729);
#11484=AXIS2_PLACEMENT_3D('',#16074,#12730,#12731);
#11485=AXIS2_PLACEMENT_3D('',#16075,#12732,#12733);
#11486=AXIS2_PLACEMENT_3D('',#16077,#12734,#12735);
#11487=AXIS2_PLACEMENT_3D('',#16079,#12736,#12737);
#11488=AXIS2_PLACEMENT_3D('',#16081,#12738,#12739);
#11489=AXIS2_PLACEMENT_3D('',#16082,#12740,#12741);
#11490=AXIS2_PLACEMENT_3D('',#16083,#12742,#12743);
#11491=AXIS2_PLACEMENT_3D('',#16087,#12745,#12746);
#11492=AXIS2_PLACEMENT_3D('',#16088,#12747,#12748);
#11493=AXIS2_PLACEMENT_3D('',#16089,#12749,#12750);
#11494=AXIS2_PLACEMENT_3D('',#16090,#12751,#12752);
#11495=AXIS2_PLACEMENT_3D('',#16092,#12753,#12754);
#11496=AXIS2_PLACEMENT_3D('',#16093,#12755,#12756);
#11497=AXIS2_PLACEMENT_3D('',#16094,#12757,#12758);
#11498=AXIS2_PLACEMENT_3D('',#16097,#12759,#12760);
#11499=AXIS2_PLACEMENT_3D('',#16099,#12761,#12762);
#11500=AXIS2_PLACEMENT_3D('',#16100,#12763,#12764);
#11501=AXIS2_PLACEMENT_3D('',#16101,#12765,#12766);
#11502=AXIS2_PLACEMENT_3D('',#16102,#12767,#12768);
#11503=AXIS2_PLACEMENT_3D('',#16105,#12769,#12770);
#11504=AXIS2_PLACEMENT_3D('',#16107,#12772,#12773);
#11505=AXIS2_PLACEMENT_3D('',#16108,#12774,#12775);
#11506=AXIS2_PLACEMENT_3D('',#16109,#12776,#12777);
#11507=AXIS2_PLACEMENT_3D('',#16110,#12778,#12779);
#11508=AXIS2_PLACEMENT_3D('',#16112,#12780,#12781);
#11509=AXIS2_PLACEMENT_3D('',#16113,#12782,#12783);
#11510=AXIS2_PLACEMENT_3D('',#16116,#12785,#12786);
#11511=AXIS2_PLACEMENT_3D('',#16117,#12787,#12788);
#11512=AXIS2_PLACEMENT_3D('',#16119,#12789,#12790);
#11513=AXIS2_PLACEMENT_3D('',#16121,#12791,#12792);
#11514=AXIS2_PLACEMENT_3D('',#16123,#12793,#12794);
#11515=AXIS2_PLACEMENT_3D('',#16124,#12795,#12796);
#11516=AXIS2_PLACEMENT_3D('',#16125,#12797,#12798);
#11517=AXIS2_PLACEMENT_3D('',#16129,#12800,#12801);
#11518=AXIS2_PLACEMENT_3D('',#16130,#12802,#12803);
#11519=AXIS2_PLACEMENT_3D('',#16131,#12804,#12805);
#11520=AXIS2_PLACEMENT_3D('',#16132,#12806,#12807);
#11521=AXIS2_PLACEMENT_3D('',#16133,#12808,#12809);
#11522=AXIS2_PLACEMENT_3D('',#16134,#12810,#12811);
#11523=AXIS2_PLACEMENT_3D('',#16135,#12812,#12813);
#11524=AXIS2_PLACEMENT_3D('',#16137,#12814,#12815);
#11525=AXIS2_PLACEMENT_3D('',#16139,#12816,#12817);
#11526=AXIS2_PLACEMENT_3D('',#16140,#12818,#12819);
#11527=AXIS2_PLACEMENT_3D('',#16143,#12821,#12822);
#11528=AXIS2_PLACEMENT_3D('',#16144,#12823,#12824);
#11529=AXIS2_PLACEMENT_3D('',#16146,#12825,#12826);
#11530=AXIS2_PLACEMENT_3D('',#16147,#12827,#12828);
#11531=AXIS2_PLACEMENT_3D('',#16149,#12829,#12830);
#11532=AXIS2_PLACEMENT_3D('',#16151,#12831,#12832);
#11533=AXIS2_PLACEMENT_3D('',#16152,#12833,#12834);
#11534=AXIS2_PLACEMENT_3D('',#16154,#12835,#12836);
#11535=AXIS2_PLACEMENT_3D('',#16156,#12837,#12838);
#11536=AXIS2_PLACEMENT_3D('',#16157,#12839,#12840);
#11537=AXIS2_PLACEMENT_3D('',#16159,#12842,#12843);
#11538=AXIS2_PLACEMENT_3D('',#16161,#12845,#12846);
#11539=AXIS2_PLACEMENT_3D('',#16163,#12847,#12848);
#11540=AXIS2_PLACEMENT_3D('',#16165,#12849,#12850);
#11541=AXIS2_PLACEMENT_3D('',#16166,#12851,#12852);
#11542=AXIS2_PLACEMENT_3D('',#16168,#12853,#12854);
#11543=AXIS2_PLACEMENT_3D('',#16170,#12856,#12857);
#11544=AXIS2_PLACEMENT_3D('',#16172,#12858,#12859);
#11545=AXIS2_PLACEMENT_3D('',#16173,#12860,#12861);
#11546=AXIS2_PLACEMENT_3D('',#16176,#12863,#12864);
#11547=AXIS2_PLACEMENT_3D('',#16177,#12865,#12866);
#11548=AXIS2_PLACEMENT_3D('',#16179,#12867,#12868);
#11549=AXIS2_PLACEMENT_3D('',#16181,#12870,#12871);
#11550=AXIS2_PLACEMENT_3D('',#16183,#12873,#12874);
#11551=AXIS2_PLACEMENT_3D('',#16185,#12875,#12876);
#11552=AXIS2_PLACEMENT_3D('',#16186,#12877,#12878);
#11553=AXIS2_PLACEMENT_3D('',#16188,#12879,#12880);
#11554=AXIS2_PLACEMENT_3D('',#16190,#12882,#12883);
#11555=AXIS2_PLACEMENT_3D('',#16191,#12884,#12885);
#11556=AXIS2_PLACEMENT_3D('',#16192,#12886,#12887);
#11557=AXIS2_PLACEMENT_3D('',#16195,#12888,#12889);
#11558=AXIS2_PLACEMENT_3D('',#16199,#12891,#12892);
#11559=AXIS2_PLACEMENT_3D('',#16201,#12894,#12895);
#11560=AXIS2_PLACEMENT_3D('',#16208,#12899,#12900);
#11561=AXIS2_PLACEMENT_3D('',#16210,#12901,#12902);
#11562=AXIS2_PLACEMENT_3D('',#16212,#12903,#12904);
#11563=AXIS2_PLACEMENT_3D('',#16214,#12905,#12906);
#11564=AXIS2_PLACEMENT_3D('',#16216,#12907,#12908);
#11565=AXIS2_PLACEMENT_3D('',#16218,#12909,#12910);
#11566=AXIS2_PLACEMENT_3D('',#16220,#12911,#12912);
#11567=AXIS2_PLACEMENT_3D('',#16222,#12913,#12914);
#11568=AXIS2_PLACEMENT_3D('',#16224,#12915,#12916);
#11569=AXIS2_PLACEMENT_3D('',#16226,#12917,#12918);
#11570=AXIS2_PLACEMENT_3D('',#16228,#12919,#12920);
#11571=AXIS2_PLACEMENT_3D('',#16229,#12921,#12922);
#11572=AXIS2_PLACEMENT_3D('',#16244,#12930,#12931);
#11573=AXIS2_PLACEMENT_3D('',#16245,#12932,#12933);
#11574=AXIS2_PLACEMENT_3D('',#16247,#12934,#12935);
#11575=AXIS2_PLACEMENT_3D('',#16249,#12937,#12938);
#11576=AXIS2_PLACEMENT_3D('',#16251,#12939,#12940);
#11577=AXIS2_PLACEMENT_3D('',#16254,#12942,#12943);
#11578=AXIS2_PLACEMENT_3D('',#16255,#12944,#12945);
#11579=AXIS2_PLACEMENT_3D('',#16257,#12946,#12947);
#11580=AXIS2_PLACEMENT_3D('',#16260,#12949,#12950);
#11581=AXIS2_PLACEMENT_3D('',#16261,#12951,#12952);
#11582=AXIS2_PLACEMENT_3D('',#16263,#12953,#12954);
#11583=AXIS2_PLACEMENT_3D('',#16266,#12956,#12957);
#11584=AXIS2_PLACEMENT_3D('',#16267,#12958,#12959);
#11585=AXIS2_PLACEMENT_3D('',#16269,#12960,#12961);
#11586=AXIS2_PLACEMENT_3D('',#16272,#12963,#12964);
#11587=AXIS2_PLACEMENT_3D('',#16273,#12965,#12966);
#11588=AXIS2_PLACEMENT_3D('',#16275,#12967,#12968);
#11589=AXIS2_PLACEMENT_3D('',#16278,#12970,#12971);
#11590=AXIS2_PLACEMENT_3D('',#16279,#12972,#12973);
#11591=AXIS2_PLACEMENT_3D('',#16281,#12974,#12975);
#11592=AXIS2_PLACEMENT_3D('',#16284,#12977,#12978);
#11593=AXIS2_PLACEMENT_3D('',#16285,#12979,#12980);
#11594=AXIS2_PLACEMENT_3D('',#16287,#12981,#12982);
#11595=AXIS2_PLACEMENT_3D('',#16290,#12984,#12985);
#11596=AXIS2_PLACEMENT_3D('',#16291,#12986,#12987);
#11597=AXIS2_PLACEMENT_3D('',#16293,#12988,#12989);
#11598=AXIS2_PLACEMENT_3D('',#16296,#12991,#12992);
#11599=AXIS2_PLACEMENT_3D('',#16297,#12993,#12994);
#11600=AXIS2_PLACEMENT_3D('',#16299,#12995,#12996);
#11601=AXIS2_PLACEMENT_3D('',#16302,#12998,#12999);
#11602=AXIS2_PLACEMENT_3D('',#16303,#13000,#13001);
#11603=AXIS2_PLACEMENT_3D('',#16305,#13002,#13003);
#11604=AXIS2_PLACEMENT_3D('',#16308,#13005,#13006);
#11605=AXIS2_PLACEMENT_3D('',#16309,#13007,#13008);
#11606=AXIS2_PLACEMENT_3D('',#16311,#13009,#13010);
#11607=AXIS2_PLACEMENT_3D('',#16314,#13012,#13013);
#11608=AXIS2_PLACEMENT_3D('',#16315,#13014,#13015);
#11609=AXIS2_PLACEMENT_3D('',#16318,#13017,#13018);
#11610=AXIS2_PLACEMENT_3D('',#16319,#13019,#13020);
#11611=AXIS2_PLACEMENT_3D('',#16322,#13022,#13023);
#11612=AXIS2_PLACEMENT_3D('',#16323,#13024,#13025);
#11613=AXIS2_PLACEMENT_3D('',#16326,#13027,#13028);
#11614=AXIS2_PLACEMENT_3D('',#16327,#13029,#13030);
#11615=AXIS2_PLACEMENT_3D('',#16330,#13032,#13033);
#11616=AXIS2_PLACEMENT_3D('',#16331,#13034,#13035);
#11617=AXIS2_PLACEMENT_3D('',#16334,#13037,#13038);
#11618=AXIS2_PLACEMENT_3D('',#16335,#13039,#13040);
#11619=AXIS2_PLACEMENT_3D('',#16338,#13042,#13043);
#11620=AXIS2_PLACEMENT_3D('',#16339,#13044,#13045);
#11621=AXIS2_PLACEMENT_3D('',#16342,#13047,#13048);
#11622=AXIS2_PLACEMENT_3D('',#16343,#13049,#13050);
#11623=AXIS2_PLACEMENT_3D('',#16346,#13052,#13053);
#11624=AXIS2_PLACEMENT_3D('',#16347,#13054,#13055);
#11625=AXIS2_PLACEMENT_3D('',#16350,#13057,#13058);
#11626=AXIS2_PLACEMENT_3D('',#16351,#13059,#13060);
#11627=AXIS2_PLACEMENT_3D('',#16354,#13062,#13063);
#11628=AXIS2_PLACEMENT_3D('',#16355,#13064,#13065);
#11629=AXIS2_PLACEMENT_3D('',#16358,#13067,#13068);
#11630=AXIS2_PLACEMENT_3D('',#16359,#13069,#13070);
#11631=AXIS2_PLACEMENT_3D('',#16361,#13071,#13072);
#11632=AXIS2_PLACEMENT_3D('',#16364,#13074,#13075);
#11633=AXIS2_PLACEMENT_3D('',#16365,#13076,#13077);
#11634=AXIS2_PLACEMENT_3D('',#16367,#13078,#13079);
#11635=AXIS2_PLACEMENT_3D('',#16370,#13081,#13082);
#11636=AXIS2_PLACEMENT_3D('',#16371,#13083,#13084);
#11637=AXIS2_PLACEMENT_3D('',#16373,#13085,#13086);
#11638=AXIS2_PLACEMENT_3D('',#16376,#13088,#13089);
#11639=AXIS2_PLACEMENT_3D('',#16377,#13090,#13091);
#11640=AXIS2_PLACEMENT_3D('',#16379,#13092,#13093);
#11641=AXIS2_PLACEMENT_3D('',#16382,#13095,#13096);
#11642=AXIS2_PLACEMENT_3D('',#16383,#13097,#13098);
#11643=AXIS2_PLACEMENT_3D('',#16385,#13099,#13100);
#11644=AXIS2_PLACEMENT_3D('',#16388,#13102,#13103);
#11645=AXIS2_PLACEMENT_3D('',#16389,#13104,#13105);
#11646=AXIS2_PLACEMENT_3D('',#16391,#13106,#13107);
#11647=AXIS2_PLACEMENT_3D('',#16394,#13109,#13110);
#11648=AXIS2_PLACEMENT_3D('',#16395,#13111,#13112);
#11649=AXIS2_PLACEMENT_3D('',#16397,#13113,#13114);
#11650=AXIS2_PLACEMENT_3D('',#16400,#13116,#13117);
#11651=AXIS2_PLACEMENT_3D('',#16401,#13118,#13119);
#11652=AXIS2_PLACEMENT_3D('',#16403,#13120,#13121);
#11653=AXIS2_PLACEMENT_3D('',#16406,#13123,#13124);
#11654=AXIS2_PLACEMENT_3D('',#16407,#13125,#13126);
#11655=AXIS2_PLACEMENT_3D('',#16409,#13127,#13128);
#11656=AXIS2_PLACEMENT_3D('',#16412,#13130,#13131);
#11657=AXIS2_PLACEMENT_3D('',#16413,#13132,#13133);
#11658=AXIS2_PLACEMENT_3D('',#16415,#13134,#13135);
#11659=AXIS2_PLACEMENT_3D('',#16418,#13137,#13138);
#11660=AXIS2_PLACEMENT_3D('',#16419,#13139,#13140);
#11661=AXIS2_PLACEMENT_3D('',#16421,#13141,#13142);
#11662=AXIS2_PLACEMENT_3D('',#16424,#13144,#13145);
#11663=AXIS2_PLACEMENT_3D('',#16425,#13146,#13147);
#11664=AXIS2_PLACEMENT_3D('',#16431,#13151,#13152);
#11665=AXIS2_PLACEMENT_3D('',#16433,#13154,#13155);
#11666=AXIS2_PLACEMENT_3D('',#16437,#13158,#13159);
#11667=AXIS2_PLACEMENT_3D('',#16441,#13162,#13163);
#11668=AXIS2_PLACEMENT_3D('',#16445,#13166,#13167);
#11669=AXIS2_PLACEMENT_3D('',#16449,#13170,#13171);
#11670=AXIS2_PLACEMENT_3D('',#16451,#13173,#13174);
#11671=AXIS2_PLACEMENT_3D('',#16452,#13175,#13176);
#11672=AXIS2_PLACEMENT_3D('',#16453,#13177,#13178);
#11673=AXIS2_PLACEMENT_3D('',#16467,#13185,#13186);
#11674=AXIS2_PLACEMENT_3D('',#16468,#13187,#13188);
#11675=AXIS2_PLACEMENT_3D('',#16474,#13192,#13193);
#11676=AXIS2_PLACEMENT_3D('',#16478,#13196,#13197);
#11677=AXIS2_PLACEMENT_3D('',#16482,#13200,#13201);
#11678=AXIS2_PLACEMENT_3D('',#16486,#13204,#13205);
#11679=AXIS2_PLACEMENT_3D('',#16490,#13208,#13209);
#11680=AXIS2_PLACEMENT_3D('',#16492,#13211,#13212);
#11681=AXIS2_PLACEMENT_3D('',#16493,#13213,#13214);
#11682=AXIS2_PLACEMENT_3D('',#16495,#13215,#13216);
#11683=AXIS2_PLACEMENT_3D('',#16497,#13218,#13219);
#11684=AXIS2_PLACEMENT_3D('',#16498,#13220,#13221);
#11685=AXIS2_PLACEMENT_3D('',#16499,#13222,#13223);
#11686=AXIS2_PLACEMENT_3D('',#16508,#13228,#13229);
#11687=AXIS2_PLACEMENT_3D('',#16510,#13230,#13231);
#11688=AXIS2_PLACEMENT_3D('',#16513,#13233,#13234);
#11689=AXIS2_PLACEMENT_3D('',#16514,#13235,#13236);
#11690=AXIS2_PLACEMENT_3D('',#16520,#13240,#13241);
#11691=AXIS2_PLACEMENT_3D('',#16529,#13246,#13247);
#11692=AXIS2_PLACEMENT_3D('',#16531,#13248,#13249);
#11693=AXIS2_PLACEMENT_3D('',#16534,#13251,#13252);
#11694=AXIS2_PLACEMENT_3D('',#16535,#13253,#13254);
#11695=AXIS2_PLACEMENT_3D('',#16541,#13258,#13259);
#11696=AXIS2_PLACEMENT_3D('',#16543,#13260,#13261);
#11697=AXIS2_PLACEMENT_3D('',#16546,#13263,#13264);
#11698=AXIS2_PLACEMENT_3D('',#16547,#13265,#13266);
#11699=AXIS2_PLACEMENT_3D('',#16549,#13267,#13268);
#11700=AXIS2_PLACEMENT_3D('',#16551,#13269,#13270);
#11701=AXIS2_PLACEMENT_3D('',#16553,#13272,#13273);
#11702=AXIS2_PLACEMENT_3D('',#16559,#13277,#13278);
#11703=AXIS2_PLACEMENT_3D('',#16568,#13283,#13284);
#11704=AXIS2_PLACEMENT_3D('',#16570,#13285,#13286);
#11705=AXIS2_PLACEMENT_3D('',#16572,#13287,#13288);
#11706=AXIS2_PLACEMENT_3D('',#16574,#13290,#13291);
#11707=AXIS2_PLACEMENT_3D('',#16580,#13295,#13296);
#11708=AXIS2_PLACEMENT_3D('',#16589,#13301,#13302);
#11709=AXIS2_PLACEMENT_3D('',#16591,#13303,#13304);
#11710=AXIS2_PLACEMENT_3D('',#16593,#13305,#13306);
#11711=AXIS2_PLACEMENT_3D('',#16595,#13308,#13309);
#11712=AXIS2_PLACEMENT_3D('',#16601,#13313,#13314);
#11713=AXIS2_PLACEMENT_3D('',#16602,#13315,#13316);
#11714=AXIS2_PLACEMENT_3D('',#16603,#13317,#13318);
#11715=AXIS2_PLACEMENT_3D('',#16604,#13319,#13320);
#11716=AXIS2_PLACEMENT_3D('',#16610,#13324,#13325);
#11717=AXIS2_PLACEMENT_3D('',#16611,#13326,#13327);
#11718=AXIS2_PLACEMENT_3D('',#16612,#13328,#13329);
#11719=AXIS2_PLACEMENT_3D('',#16613,#13330,#13331);
#11720=AXIS2_PLACEMENT_3D('',#16619,#13335,#13336);
#11721=AXIS2_PLACEMENT_3D('',#16625,#13340,#13341);
#11722=AXIS2_PLACEMENT_3D('',#16628,#13344,#13345);
#11723=AXIS2_PLACEMENT_3D('',#16630,#13346,#13347);
#11724=AXIS2_PLACEMENT_3D('',#16633,#13349,#13350);
#11725=AXIS2_PLACEMENT_3D('',#16634,#13351,#13352);
#11726=AXIS2_PLACEMENT_3D('',#16640,#13356,#13357);
#11727=AXIS2_PLACEMENT_3D('',#16642,#13358,#13359);
#11728=AXIS2_PLACEMENT_3D('',#16645,#13361,#13362);
#11729=AXIS2_PLACEMENT_3D('',#16646,#13363,#13364);
#11730=AXIS2_PLACEMENT_3D('',#16652,#13368,#13369);
#11731=AXIS2_PLACEMENT_3D('',#16658,#13373,#13374);
#11732=AXIS2_PLACEMENT_3D('',#16664,#13378,#13379);
#11733=AXIS2_PLACEMENT_3D('',#16666,#13380,#13381);
#11734=AXIS2_PLACEMENT_3D('',#16669,#13383,#13384);
#11735=AXIS2_PLACEMENT_3D('',#16670,#13385,#13386);
#11736=AXIS2_PLACEMENT_3D('',#16676,#13390,#13391);
#11737=AXIS2_PLACEMENT_3D('',#16678,#13392,#13393);
#11738=AXIS2_PLACEMENT_3D('',#16681,#13395,#13396);
#11739=AXIS2_PLACEMENT_3D('',#16682,#13397,#13398);
#11740=AXIS2_PLACEMENT_3D('',#16688,#13402,#13403);
#11741=AXIS2_PLACEMENT_3D('',#16690,#13404,#13405);
#11742=AXIS2_PLACEMENT_3D('',#16692,#13406,#13407);
#11743=AXIS2_PLACEMENT_3D('',#16694,#13409,#13410);
#11744=AXIS2_PLACEMENT_3D('',#16700,#13414,#13415);
#11745=AXIS2_PLACEMENT_3D('',#16702,#13416,#13417);
#11746=AXIS2_PLACEMENT_3D('',#16704,#13418,#13419);
#11747=AXIS2_PLACEMENT_3D('',#16706,#13421,#13422);
#11748=AXIS2_PLACEMENT_3D('',#16712,#13426,#13427);
#11749=AXIS2_PLACEMENT_3D('',#16718,#13431,#13432);
#11750=AXIS2_PLACEMENT_3D('',#16724,#13436,#13437);
#11751=AXIS2_PLACEMENT_3D('',#16726,#13438,#13439);
#11752=AXIS2_PLACEMENT_3D('',#16728,#13440,#13441);
#11753=AXIS2_PLACEMENT_3D('',#16730,#13443,#13444);
#11754=AXIS2_PLACEMENT_3D('',#16736,#13448,#13449);
#11755=AXIS2_PLACEMENT_3D('',#16737,#13450,#13451);
#11756=AXIS2_PLACEMENT_3D('',#16738,#13452,#13453);
#11757=AXIS2_PLACEMENT_3D('',#16739,#13454,#13455);
#11758=AXIS2_PLACEMENT_3D('',#16740,#13456,#13457);
#11759=AXIS2_PLACEMENT_3D('',#16741,#13458,#13459);
#11760=AXIS2_PLACEMENT_3D('',#16742,#13460,#13461);
#11761=AXIS2_PLACEMENT_3D('',#16744,#13462,#13463);
#11762=AXIS2_PLACEMENT_3D('',#16747,#13465,#13466);
#11763=AXIS2_PLACEMENT_3D('',#16748,#13467,#13468);
#11764=AXIS2_PLACEMENT_3D('',#16750,#13469,#13470);
#11765=AXIS2_PLACEMENT_3D('',#16753,#13472,#13473);
#11766=AXIS2_PLACEMENT_3D('',#16754,#13474,#13475);
#11767=AXIS2_PLACEMENT_3D('',#16756,#13476,#13477);
#11768=AXIS2_PLACEMENT_3D('',#16759,#13479,#13480);
#11769=AXIS2_PLACEMENT_3D('',#16760,#13481,#13482);
#11770=AXIS2_PLACEMENT_3D('',#16762,#13483,#13484);
#11771=AXIS2_PLACEMENT_3D('',#16765,#13486,#13487);
#11772=AXIS2_PLACEMENT_3D('',#16766,#13488,#13489);
#11773=AXIS2_PLACEMENT_3D('',#16768,#13490,#13491);
#11774=AXIS2_PLACEMENT_3D('',#16771,#13493,#13494);
#11775=AXIS2_PLACEMENT_3D('',#16772,#13495,#13496);
#11776=AXIS2_PLACEMENT_3D('',#16781,#13501,#13502);
#11777=AXIS2_PLACEMENT_3D('',#16783,#13503,#13504);
#11778=AXIS2_PLACEMENT_3D('',#16785,#13505,#13506);
#11779=AXIS2_PLACEMENT_3D('',#16787,#13508,#13509);
#11780=AXIS2_PLACEMENT_3D('',#16793,#13513,#13514);
#11781=AXIS2_PLACEMENT_3D('',#16794,#13515,#13516);
#11782=AXIS2_PLACEMENT_3D('',#16795,#13517,#13518);
#11783=AXIS2_PLACEMENT_3D('',#16796,#13519,#13520);
#11784=AXIS2_PLACEMENT_3D('',#16805,#13525,#13526);
#11785=AXIS2_PLACEMENT_3D('',#16807,#13527,#13528);
#11786=AXIS2_PLACEMENT_3D('',#16809,#13529,#13530);
#11787=AXIS2_PLACEMENT_3D('',#16811,#13532,#13533);
#11788=AXIS2_PLACEMENT_3D('',#16817,#13537,#13538);
#11789=AXIS2_PLACEMENT_3D('',#16818,#13539,#13540);
#11790=AXIS2_PLACEMENT_3D('',#16819,#13541,#13542);
#11791=AXIS2_PLACEMENT_3D('',#16820,#13543,#13544);
#11792=AXIS2_PLACEMENT_3D('',#16822,#13545,#13546);
#11793=AXIS2_PLACEMENT_3D('',#16825,#13548,#13549);
#11794=AXIS2_PLACEMENT_3D('',#16826,#13550,#13551);
#11795=AXIS2_PLACEMENT_3D('',#16828,#13552,#13553);
#11796=AXIS2_PLACEMENT_3D('',#16831,#13555,#13556);
#11797=AXIS2_PLACEMENT_3D('',#16832,#13557,#13558);
#11798=AXIS2_PLACEMENT_3D('',#16834,#13559,#13560);
#11799=AXIS2_PLACEMENT_3D('',#16837,#13562,#13563);
#11800=AXIS2_PLACEMENT_3D('',#16838,#13564,#13565);
#11801=AXIS2_PLACEMENT_3D('',#16840,#13566,#13567);
#11802=AXIS2_PLACEMENT_3D('',#16843,#13569,#13570);
#11803=AXIS2_PLACEMENT_3D('',#16844,#13571,#13572);
#11804=AXIS2_PLACEMENT_3D('',#16846,#13573,#13574);
#11805=AXIS2_PLACEMENT_3D('',#16849,#13576,#13577);
#11806=AXIS2_PLACEMENT_3D('',#16850,#13578,#13579);
#11807=AXIS2_PLACEMENT_3D('',#16859,#13584,#13585);
#11808=AXIS2_PLACEMENT_3D('',#16861,#13586,#13587);
#11809=AXIS2_PLACEMENT_3D('',#16863,#13588,#13589);
#11810=AXIS2_PLACEMENT_3D('',#16865,#13591,#13592);
#11811=AXIS2_PLACEMENT_3D('',#16871,#13596,#13597);
#11812=AXIS2_PLACEMENT_3D('',#16872,#13598,#13599);
#11813=AXIS2_PLACEMENT_3D('',#16873,#13600,#13601);
#11814=AXIS2_PLACEMENT_3D('',#16874,#13602,#13603);
#11815=AXIS2_PLACEMENT_3D('',#16883,#13608,#13609);
#11816=AXIS2_PLACEMENT_3D('',#16885,#13610,#13611);
#11817=AXIS2_PLACEMENT_3D('',#16887,#13612,#13613);
#11818=AXIS2_PLACEMENT_3D('',#16889,#13615,#13616);
#11819=AXIS2_PLACEMENT_3D('',#16895,#13620,#13621);
#11820=AXIS2_PLACEMENT_3D('',#16896,#13622,#13623);
#11821=AXIS2_PLACEMENT_3D('',#16897,#13624,#13625);
#11822=AXIS2_PLACEMENT_3D('',#16898,#13626,#13627);
#11823=AXIS2_PLACEMENT_3D('',#16900,#13628,#13629);
#11824=AXIS2_PLACEMENT_3D('',#16903,#13631,#13632);
#11825=AXIS2_PLACEMENT_3D('',#16904,#13633,#13634);
#11826=AXIS2_PLACEMENT_3D('',#16906,#13635,#13636);
#11827=AXIS2_PLACEMENT_3D('',#16909,#13638,#13639);
#11828=AXIS2_PLACEMENT_3D('',#16910,#13640,#13641);
#11829=AXIS2_PLACEMENT_3D('',#16912,#13642,#13643);
#11830=AXIS2_PLACEMENT_3D('',#16915,#13645,#13646);
#11831=AXIS2_PLACEMENT_3D('',#16916,#13647,#13648);
#11832=AXIS2_PLACEMENT_3D('',#16918,#13649,#13650);
#11833=AXIS2_PLACEMENT_3D('',#16921,#13652,#13653);
#11834=AXIS2_PLACEMENT_3D('',#16922,#13654,#13655);
#11835=AXIS2_PLACEMENT_3D('',#16924,#13656,#13657);
#11836=AXIS2_PLACEMENT_3D('',#16927,#13659,#13660);
#11837=AXIS2_PLACEMENT_3D('',#16928,#13661,#13662);
#11838=AXIS2_PLACEMENT_3D('',#16937,#13667,#13668);
#11839=AXIS2_PLACEMENT_3D('',#16939,#13669,#13670);
#11840=AXIS2_PLACEMENT_3D('',#16941,#13671,#13672);
#11841=AXIS2_PLACEMENT_3D('',#16943,#13674,#13675);
#11842=AXIS2_PLACEMENT_3D('',#16949,#13679,#13680);
#11843=AXIS2_PLACEMENT_3D('',#16950,#13681,#13682);
#11844=AXIS2_PLACEMENT_3D('',#16951,#13683,#13684);
#11845=AXIS2_PLACEMENT_3D('',#16952,#13685,#13686);
#11846=AXIS2_PLACEMENT_3D('',#16961,#13691,#13692);
#11847=AXIS2_PLACEMENT_3D('',#16963,#13693,#13694);
#11848=AXIS2_PLACEMENT_3D('',#16965,#13695,#13696);
#11849=AXIS2_PLACEMENT_3D('',#16967,#13698,#13699);
#11850=AXIS2_PLACEMENT_3D('',#16973,#13703,#13704);
#11851=AXIS2_PLACEMENT_3D('',#16974,#13705,#13706);
#11852=AXIS2_PLACEMENT_3D('',#16975,#13707,#13708);
#11853=AXIS2_PLACEMENT_3D('',#16976,#13709,#13710);
#11854=AXIS2_PLACEMENT_3D('',#16978,#13711,#13712);
#11855=AXIS2_PLACEMENT_3D('',#16981,#13714,#13715);
#11856=AXIS2_PLACEMENT_3D('',#16982,#13716,#13717);
#11857=AXIS2_PLACEMENT_3D('',#16984,#13718,#13719);
#11858=AXIS2_PLACEMENT_3D('',#16987,#13721,#13722);
#11859=AXIS2_PLACEMENT_3D('',#16988,#13723,#13724);
#11860=AXIS2_PLACEMENT_3D('',#16990,#13725,#13726);
#11861=AXIS2_PLACEMENT_3D('',#16993,#13728,#13729);
#11862=AXIS2_PLACEMENT_3D('',#16994,#13730,#13731);
#11863=AXIS2_PLACEMENT_3D('',#16996,#13732,#13733);
#11864=AXIS2_PLACEMENT_3D('',#16999,#13735,#13736);
#11865=AXIS2_PLACEMENT_3D('',#17000,#13737,#13738);
#11866=AXIS2_PLACEMENT_3D('',#17002,#13739,#13740);
#11867=AXIS2_PLACEMENT_3D('',#17005,#13742,#13743);
#11868=AXIS2_PLACEMENT_3D('',#17006,#13744,#13745);
#11869=AXIS2_PLACEMENT_3D('',#17015,#13750,#13751);
#11870=AXIS2_PLACEMENT_3D('',#17017,#13752,#13753);
#11871=AXIS2_PLACEMENT_3D('',#17019,#13754,#13755);
#11872=AXIS2_PLACEMENT_3D('',#17021,#13757,#13758);
#11873=AXIS2_PLACEMENT_3D('',#17027,#13762,#13763);
#11874=AXIS2_PLACEMENT_3D('',#17028,#13764,#13765);
#11875=AXIS2_PLACEMENT_3D('',#17029,#13766,#13767);
#11876=AXIS2_PLACEMENT_3D('',#17030,#13768,#13769);
#11877=AXIS2_PLACEMENT_3D('',#17039,#13774,#13775);
#11878=AXIS2_PLACEMENT_3D('',#17041,#13776,#13777);
#11879=AXIS2_PLACEMENT_3D('',#17043,#13778,#13779);
#11880=AXIS2_PLACEMENT_3D('',#17045,#13781,#13782);
#11881=AXIS2_PLACEMENT_3D('',#17051,#13786,#13787);
#11882=AXIS2_PLACEMENT_3D('',#17052,#13788,#13789);
#11883=AXIS2_PLACEMENT_3D('',#17053,#13790,#13791);
#11884=AXIS2_PLACEMENT_3D('',#17054,#13792,#13793);
#11885=AXIS2_PLACEMENT_3D('',#17056,#13794,#13795);
#11886=AXIS2_PLACEMENT_3D('',#17059,#13797,#13798);
#11887=AXIS2_PLACEMENT_3D('',#17060,#13799,#13800);
#11888=AXIS2_PLACEMENT_3D('',#17062,#13801,#13802);
#11889=AXIS2_PLACEMENT_3D('',#17065,#13804,#13805);
#11890=AXIS2_PLACEMENT_3D('',#17066,#13806,#13807);
#11891=AXIS2_PLACEMENT_3D('',#17068,#13808,#13809);
#11892=AXIS2_PLACEMENT_3D('',#17071,#13811,#13812);
#11893=AXIS2_PLACEMENT_3D('',#17072,#13813,#13814);
#11894=AXIS2_PLACEMENT_3D('',#17074,#13815,#13816);
#11895=AXIS2_PLACEMENT_3D('',#17077,#13818,#13819);
#11896=AXIS2_PLACEMENT_3D('',#17078,#13820,#13821);
#11897=AXIS2_PLACEMENT_3D('',#17080,#13822,#13823);
#11898=AXIS2_PLACEMENT_3D('',#17083,#13825,#13826);
#11899=AXIS2_PLACEMENT_3D('',#17084,#13827,#13828);
#11900=AXIS2_PLACEMENT_3D('',#17093,#13833,#13834);
#11901=AXIS2_PLACEMENT_3D('',#17095,#13835,#13836);
#11902=AXIS2_PLACEMENT_3D('',#17097,#13837,#13838);
#11903=AXIS2_PLACEMENT_3D('',#17099,#13840,#13841);
#11904=AXIS2_PLACEMENT_3D('',#17105,#13845,#13846);
#11905=AXIS2_PLACEMENT_3D('',#17106,#13847,#13848);
#11906=AXIS2_PLACEMENT_3D('',#17107,#13849,#13850);
#11907=AXIS2_PLACEMENT_3D('',#17108,#13851,#13852);
#11908=AXIS2_PLACEMENT_3D('',#17117,#13857,#13858);
#11909=AXIS2_PLACEMENT_3D('',#17119,#13859,#13860);
#11910=AXIS2_PLACEMENT_3D('',#17121,#13861,#13862);
#11911=AXIS2_PLACEMENT_3D('',#17123,#13864,#13865);
#11912=AXIS2_PLACEMENT_3D('',#17129,#13869,#13870);
#11913=AXIS2_PLACEMENT_3D('',#17130,#13871,#13872);
#11914=AXIS2_PLACEMENT_3D('',#17131,#13873,#13874);
#11915=AXIS2_PLACEMENT_3D('',#17132,#13875,#13876);
#11916=AXIS2_PLACEMENT_3D('',#17134,#13877,#13878);
#11917=AXIS2_PLACEMENT_3D('',#17137,#13880,#13881);
#11918=AXIS2_PLACEMENT_3D('',#17138,#13882,#13883);
#11919=AXIS2_PLACEMENT_3D('',#17140,#13884,#13885);
#11920=AXIS2_PLACEMENT_3D('',#17143,#13887,#13888);
#11921=AXIS2_PLACEMENT_3D('',#17144,#13889,#13890);
#11922=AXIS2_PLACEMENT_3D('',#17146,#13891,#13892);
#11923=AXIS2_PLACEMENT_3D('',#17149,#13894,#13895);
#11924=AXIS2_PLACEMENT_3D('',#17150,#13896,#13897);
#11925=AXIS2_PLACEMENT_3D('',#17152,#13898,#13899);
#11926=AXIS2_PLACEMENT_3D('',#17155,#13901,#13902);
#11927=AXIS2_PLACEMENT_3D('',#17156,#13903,#13904);
#11928=AXIS2_PLACEMENT_3D('',#17158,#13905,#13906);
#11929=AXIS2_PLACEMENT_3D('',#17161,#13908,#13909);
#11930=AXIS2_PLACEMENT_3D('',#17162,#13910,#13911);
#11931=AXIS2_PLACEMENT_3D('',#17171,#13916,#13917);
#11932=AXIS2_PLACEMENT_3D('',#17173,#13918,#13919);
#11933=AXIS2_PLACEMENT_3D('',#17175,#13920,#13921);
#11934=AXIS2_PLACEMENT_3D('',#17177,#13923,#13924);
#11935=AXIS2_PLACEMENT_3D('',#17183,#13928,#13929);
#11936=AXIS2_PLACEMENT_3D('',#17184,#13930,#13931);
#11937=AXIS2_PLACEMENT_3D('',#17185,#13932,#13933);
#11938=AXIS2_PLACEMENT_3D('',#17186,#13934,#13935);
#11939=AXIS2_PLACEMENT_3D('',#17195,#13940,#13941);
#11940=AXIS2_PLACEMENT_3D('',#17197,#13942,#13943);
#11941=AXIS2_PLACEMENT_3D('',#17199,#13944,#13945);
#11942=AXIS2_PLACEMENT_3D('',#17201,#13947,#13948);
#11943=AXIS2_PLACEMENT_3D('',#17207,#13952,#13953);
#11944=AXIS2_PLACEMENT_3D('',#17208,#13954,#13955);
#11945=AXIS2_PLACEMENT_3D('',#17209,#13956,#13957);
#11946=AXIS2_PLACEMENT_3D('',#17210,#13958,#13959);
#11947=AXIS2_PLACEMENT_3D('',#17212,#13960,#13961);
#11948=AXIS2_PLACEMENT_3D('',#17215,#13963,#13964);
#11949=AXIS2_PLACEMENT_3D('',#17216,#13965,#13966);
#11950=AXIS2_PLACEMENT_3D('',#17218,#13967,#13968);
#11951=AXIS2_PLACEMENT_3D('',#17221,#13970,#13971);
#11952=AXIS2_PLACEMENT_3D('',#17222,#13972,#13973);
#11953=AXIS2_PLACEMENT_3D('',#17224,#13974,#13975);
#11954=AXIS2_PLACEMENT_3D('',#17227,#13977,#13978);
#11955=AXIS2_PLACEMENT_3D('',#17228,#13979,#13980);
#11956=AXIS2_PLACEMENT_3D('',#17230,#13981,#13982);
#11957=AXIS2_PLACEMENT_3D('',#17233,#13984,#13985);
#11958=AXIS2_PLACEMENT_3D('',#17234,#13986,#13987);
#11959=AXIS2_PLACEMENT_3D('',#17236,#13988,#13989);
#11960=AXIS2_PLACEMENT_3D('',#17239,#13991,#13992);
#11961=AXIS2_PLACEMENT_3D('',#17240,#13993,#13994);
#11962=AXIS2_PLACEMENT_3D('',#17249,#13999,#14000);
#11963=AXIS2_PLACEMENT_3D('',#17251,#14001,#14002);
#11964=AXIS2_PLACEMENT_3D('',#17253,#14003,#14004);
#11965=AXIS2_PLACEMENT_3D('',#17255,#14006,#14007);
#11966=AXIS2_PLACEMENT_3D('',#17261,#14011,#14012);
#11967=AXIS2_PLACEMENT_3D('',#17262,#14013,#14014);
#11968=AXIS2_PLACEMENT_3D('',#17263,#14015,#14016);
#11969=AXIS2_PLACEMENT_3D('',#17264,#14017,#14018);
#11970=AXIS2_PLACEMENT_3D('',#17273,#14023,#14024);
#11971=AXIS2_PLACEMENT_3D('',#17275,#14025,#14026);
#11972=AXIS2_PLACEMENT_3D('',#17277,#14027,#14028);
#11973=AXIS2_PLACEMENT_3D('',#17279,#14030,#14031);
#11974=AXIS2_PLACEMENT_3D('',#17285,#14035,#14036);
#11975=AXIS2_PLACEMENT_3D('',#17286,#14037,#14038);
#11976=AXIS2_PLACEMENT_3D('',#17287,#14039,#14040);
#11977=AXIS2_PLACEMENT_3D('',#17288,#14041,#14042);
#11978=AXIS2_PLACEMENT_3D('',#17290,#14043,#14044);
#11979=AXIS2_PLACEMENT_3D('',#17293,#14046,#14047);
#11980=AXIS2_PLACEMENT_3D('',#17294,#14048,#14049);
#11981=AXIS2_PLACEMENT_3D('',#17296,#14050,#14051);
#11982=AXIS2_PLACEMENT_3D('',#17299,#14053,#14054);
#11983=AXIS2_PLACEMENT_3D('',#17300,#14055,#14056);
#11984=AXIS2_PLACEMENT_3D('',#17302,#14057,#14058);
#11985=AXIS2_PLACEMENT_3D('',#17305,#14060,#14061);
#11986=AXIS2_PLACEMENT_3D('',#17306,#14062,#14063);
#11987=AXIS2_PLACEMENT_3D('',#17308,#14064,#14065);
#11988=AXIS2_PLACEMENT_3D('',#17311,#14067,#14068);
#11989=AXIS2_PLACEMENT_3D('',#17312,#14069,#14070);
#11990=AXIS2_PLACEMENT_3D('',#17314,#14071,#14072);
#11991=AXIS2_PLACEMENT_3D('',#17317,#14074,#14075);
#11992=AXIS2_PLACEMENT_3D('',#17318,#14076,#14077);
#11993=AXIS2_PLACEMENT_3D('',#17327,#14082,#14083);
#11994=AXIS2_PLACEMENT_3D('',#17329,#14084,#14085);
#11995=AXIS2_PLACEMENT_3D('',#17331,#14086,#14087);
#11996=AXIS2_PLACEMENT_3D('',#17333,#14089,#14090);
#11997=AXIS2_PLACEMENT_3D('',#17339,#14094,#14095);
#11998=AXIS2_PLACEMENT_3D('',#17340,#14096,#14097);
#11999=AXIS2_PLACEMENT_3D('',#17341,#14098,#14099);
#12000=AXIS2_PLACEMENT_3D('',#17342,#14100,#14101);
#12001=AXIS2_PLACEMENT_3D('',#17351,#14106,#14107);
#12002=AXIS2_PLACEMENT_3D('',#17353,#14108,#14109);
#12003=AXIS2_PLACEMENT_3D('',#17355,#14110,#14111);
#12004=AXIS2_PLACEMENT_3D('',#17357,#14113,#14114);
#12005=AXIS2_PLACEMENT_3D('',#17363,#14118,#14119);
#12006=AXIS2_PLACEMENT_3D('',#17364,#14120,#14121);
#12007=AXIS2_PLACEMENT_3D('',#17365,#14122,#14123);
#12008=AXIS2_PLACEMENT_3D('',#17366,#14124,#14125);
#12009=AXIS2_PLACEMENT_3D('',#17368,#14126,#14127);
#12010=AXIS2_PLACEMENT_3D('',#17371,#14129,#14130);
#12011=AXIS2_PLACEMENT_3D('',#17372,#14131,#14132);
#12012=AXIS2_PLACEMENT_3D('',#17374,#14133,#14134);
#12013=AXIS2_PLACEMENT_3D('',#17377,#14136,#14137);
#12014=AXIS2_PLACEMENT_3D('',#17378,#14138,#14139);
#12015=AXIS2_PLACEMENT_3D('',#17380,#14140,#14141);
#12016=AXIS2_PLACEMENT_3D('',#17383,#14143,#14144);
#12017=AXIS2_PLACEMENT_3D('',#17384,#14145,#14146);
#12018=AXIS2_PLACEMENT_3D('',#17386,#14147,#14148);
#12019=AXIS2_PLACEMENT_3D('',#17389,#14150,#14151);
#12020=AXIS2_PLACEMENT_3D('',#17390,#14152,#14153);
#12021=AXIS2_PLACEMENT_3D('',#17392,#14154,#14155);
#12022=AXIS2_PLACEMENT_3D('',#17395,#14157,#14158);
#12023=AXIS2_PLACEMENT_3D('',#17396,#14159,#14160);
#12024=AXIS2_PLACEMENT_3D('',#17405,#14165,#14166);
#12025=AXIS2_PLACEMENT_3D('',#17407,#14167,#14168);
#12026=AXIS2_PLACEMENT_3D('',#17409,#14169,#14170);
#12027=AXIS2_PLACEMENT_3D('',#17411,#14172,#14173);
#12028=AXIS2_PLACEMENT_3D('',#17417,#14177,#14178);
#12029=AXIS2_PLACEMENT_3D('',#17418,#14179,#14180);
#12030=AXIS2_PLACEMENT_3D('',#17419,#14181,#14182);
#12031=AXIS2_PLACEMENT_3D('',#17420,#14183,#14184);
#12032=AXIS2_PLACEMENT_3D('',#17429,#14189,#14190);
#12033=AXIS2_PLACEMENT_3D('',#17431,#14191,#14192);
#12034=AXIS2_PLACEMENT_3D('',#17433,#14193,#14194);
#12035=AXIS2_PLACEMENT_3D('',#17435,#14196,#14197);
#12036=AXIS2_PLACEMENT_3D('',#17441,#14201,#14202);
#12037=AXIS2_PLACEMENT_3D('',#17442,#14203,#14204);
#12038=AXIS2_PLACEMENT_3D('',#17443,#14205,#14206);
#12039=AXIS2_PLACEMENT_3D('',#17444,#14207,#14208);
#12040=AXIS2_PLACEMENT_3D('',#17446,#14209,#14210);
#12041=AXIS2_PLACEMENT_3D('',#17449,#14212,#14213);
#12042=AXIS2_PLACEMENT_3D('',#17450,#14214,#14215);
#12043=AXIS2_PLACEMENT_3D('',#17452,#14216,#14217);
#12044=AXIS2_PLACEMENT_3D('',#17455,#14219,#14220);
#12045=AXIS2_PLACEMENT_3D('',#17456,#14221,#14222);
#12046=AXIS2_PLACEMENT_3D('',#17465,#14227,#14228);
#12047=AXIS2_PLACEMENT_3D('',#17467,#14229,#14230);
#12048=AXIS2_PLACEMENT_3D('',#17469,#14231,#14232);
#12049=AXIS2_PLACEMENT_3D('',#17471,#14234,#14235);
#12050=AXIS2_PLACEMENT_3D('',#17477,#14239,#14240);
#12051=AXIS2_PLACEMENT_3D('',#17478,#14241,#14242);
#12052=AXIS2_PLACEMENT_3D('',#17479,#14243,#14244);
#12053=AXIS2_PLACEMENT_3D('',#17480,#14245,#14246);
#12054=AXIS2_PLACEMENT_3D('',#17489,#14251,#14252);
#12055=AXIS2_PLACEMENT_3D('',#17491,#14253,#14254);
#12056=AXIS2_PLACEMENT_3D('',#17493,#14255,#14256);
#12057=AXIS2_PLACEMENT_3D('',#17495,#14258,#14259);
#12058=AXIS2_PLACEMENT_3D('',#17501,#14263,#14264);
#12059=AXIS2_PLACEMENT_3D('',#17502,#14265,#14266);
#12060=AXIS2_PLACEMENT_3D('',#17503,#14267,#14268);
#12061=AXIS2_PLACEMENT_3D('',#17504,#14269,#14270);
#12062=AXIS2_PLACEMENT_3D('',#17506,#14271,#14272);
#12063=AXIS2_PLACEMENT_3D('',#17509,#14274,#14275);
#12064=AXIS2_PLACEMENT_3D('',#17510,#14276,#14277);
#12065=AXIS2_PLACEMENT_3D('',#17512,#14278,#14279);
#12066=AXIS2_PLACEMENT_3D('',#17515,#14281,#14282);
#12067=AXIS2_PLACEMENT_3D('',#17516,#14283,#14284);
#12068=AXIS2_PLACEMENT_3D('',#17518,#14285,#14286);
#12069=AXIS2_PLACEMENT_3D('',#17521,#14288,#14289);
#12070=AXIS2_PLACEMENT_3D('',#17522,#14290,#14291);
#12071=AXIS2_PLACEMENT_3D('',#17525,#14292,#14293);
#12072=AXIS2_PLACEMENT_3D('',#17529,#14295,#14296);
#12073=AXIS2_PLACEMENT_3D('',#17531,#14298,#14299);
#12074=AXIS2_PLACEMENT_3D('',#17537,#14303,#14304);
#12075=AXIS2_PLACEMENT_3D('',#17539,#14305,#14306);
#12076=AXIS2_PLACEMENT_3D('',#17542,#14308,#14309);
#12077=AXIS2_PLACEMENT_3D('',#17543,#14310,#14311);
#12078=AXIS2_PLACEMENT_3D('',#17550,#14315,#14316);
#12079=AXIS2_PLACEMENT_3D('',#17552,#14317,#14318);
#12080=AXIS2_PLACEMENT_3D('',#17554,#14319,#14320);
#12081=AXIS2_PLACEMENT_3D('',#17556,#14321,#14322);
#12082=AXIS2_PLACEMENT_3D('',#17558,#14323,#14324);
#12083=AXIS2_PLACEMENT_3D('',#17560,#14325,#14326);
#12084=AXIS2_PLACEMENT_3D('',#17562,#14327,#14328);
#12085=AXIS2_PLACEMENT_3D('',#17564,#14329,#14330);
#12086=AXIS2_PLACEMENT_3D('',#17566,#14331,#14332);
#12087=AXIS2_PLACEMENT_3D('',#17568,#14333,#14334);
#12088=AXIS2_PLACEMENT_3D('',#17570,#14335,#14336);
#12089=AXIS2_PLACEMENT_3D('',#17572,#14337,#14338);
#12090=AXIS2_PLACEMENT_3D('',#17574,#14339,#14340);
#12091=AXIS2_PLACEMENT_3D('',#17576,#14341,#14342);
#12092=AXIS2_PLACEMENT_3D('',#17578,#14343,#14344);
#12093=AXIS2_PLACEMENT_3D('',#17580,#14345,#14346);
#12094=AXIS2_PLACEMENT_3D('',#17582,#14347,#14348);
#12095=AXIS2_PLACEMENT_3D('',#17584,#14349,#14350);
#12096=AXIS2_PLACEMENT_3D('',#17586,#14351,#14352);
#12097=AXIS2_PLACEMENT_3D('',#17588,#14353,#14354);
#12098=AXIS2_PLACEMENT_3D('',#17590,#14355,#14356);
#12099=AXIS2_PLACEMENT_3D('',#17592,#14357,#14358);
#12100=AXIS2_PLACEMENT_3D('',#17594,#14359,#14360);
#12101=AXIS2_PLACEMENT_3D('',#17596,#14361,#14362);
#12102=AXIS2_PLACEMENT_3D('',#17598,#14363,#14364);
#12103=AXIS2_PLACEMENT_3D('',#17600,#14365,#14366);
#12104=AXIS2_PLACEMENT_3D('',#17602,#14367,#14368);
#12105=AXIS2_PLACEMENT_3D('',#17604,#14369,#14370);
#12106=AXIS2_PLACEMENT_3D('',#17606,#14371,#14372);
#12107=AXIS2_PLACEMENT_3D('',#17608,#14373,#14374);
#12108=AXIS2_PLACEMENT_3D('',#17610,#14375,#14376);
#12109=AXIS2_PLACEMENT_3D('',#17612,#14377,#14378);
#12110=AXIS2_PLACEMENT_3D('',#17614,#14379,#14380);
#12111=AXIS2_PLACEMENT_3D('',#17616,#14381,#14382);
#12112=AXIS2_PLACEMENT_3D('',#17618,#14383,#14384);
#12113=AXIS2_PLACEMENT_3D('',#17620,#14385,#14386);
#12114=AXIS2_PLACEMENT_3D('',#17622,#14387,#14388);
#12115=AXIS2_PLACEMENT_3D('',#17624,#14389,#14390);
#12116=AXIS2_PLACEMENT_3D('',#17626,#14391,#14392);
#12117=AXIS2_PLACEMENT_3D('',#17628,#14393,#14394);
#12118=AXIS2_PLACEMENT_3D('',#17630,#14395,#14396);
#12119=AXIS2_PLACEMENT_3D('',#17632,#14397,#14398);
#12120=AXIS2_PLACEMENT_3D('',#17634,#14399,#14400);
#12121=AXIS2_PLACEMENT_3D('',#17636,#14401,#14402);
#12122=AXIS2_PLACEMENT_3D('',#17638,#14403,#14404);
#12123=AXIS2_PLACEMENT_3D('',#17640,#14405,#14406);
#12124=AXIS2_PLACEMENT_3D('',#17642,#14407,#14408);
#12125=AXIS2_PLACEMENT_3D('',#17643,#14409,#14410);
#12126=AXIS2_PLACEMENT_3D('',#17646,#14411,#14412);
#12127=AXIS2_PLACEMENT_3D('',#17650,#14414,#14415);
#12128=AXIS2_PLACEMENT_3D('',#17652,#14417,#14418);
#12129=AXIS2_PLACEMENT_3D('',#17658,#14422,#14423);
#12130=AXIS2_PLACEMENT_3D('',#17668,#14429,#14430);
#12131=AXIS2_PLACEMENT_3D('',#17669,#14431,#14432);
#12132=AXIS2_PLACEMENT_3D('',#17671,#14433,#14434);
#12133=AXIS2_PLACEMENT_3D('',#17673,#14436,#14437);
#12134=AXIS2_PLACEMENT_3D('',#17675,#14438,#14439);
#12135=AXIS2_PLACEMENT_3D('',#17677,#14441,#14442);
#12136=AXIS2_PLACEMENT_3D('',#17679,#14443,#14444);
#12137=AXIS2_PLACEMENT_3D('',#17681,#14446,#14447);
#12138=AXIS2_PLACEMENT_3D('',#17683,#14448,#14449);
#12139=AXIS2_PLACEMENT_3D('',#17685,#14451,#14452);
#12140=AXIS2_PLACEMENT_3D('',#17687,#14453,#14454);
#12141=AXIS2_PLACEMENT_3D('',#17689,#14456,#14457);
#12142=AXIS2_PLACEMENT_3D('',#17691,#14458,#14459);
#12143=AXIS2_PLACEMENT_3D('',#17693,#14461,#14462);
#12144=AXIS2_PLACEMENT_3D('',#17695,#14463,#14464);
#12145=AXIS2_PLACEMENT_3D('',#17697,#14466,#14467);
#12146=AXIS2_PLACEMENT_3D('',#17699,#14468,#14469);
#12147=AXIS2_PLACEMENT_3D('',#17701,#14471,#14472);
#12148=AXIS2_PLACEMENT_3D('',#17703,#14473,#14474);
#12149=AXIS2_PLACEMENT_3D('',#17705,#14476,#14477);
#12150=AXIS2_PLACEMENT_3D('',#17707,#14478,#14479);
#12151=AXIS2_PLACEMENT_3D('',#17709,#14481,#14482);
#12152=AXIS2_PLACEMENT_3D('',#17711,#14483,#14484);
#12153=AXIS2_PLACEMENT_3D('',#17713,#14486,#14487);
#12154=AXIS2_PLACEMENT_3D('',#17715,#14488,#14489);
#12155=AXIS2_PLACEMENT_3D('',#17717,#14491,#14492);
#12156=AXIS2_PLACEMENT_3D('',#17719,#14493,#14494);
#12157=AXIS2_PLACEMENT_3D('',#17721,#14496,#14497);
#12158=AXIS2_PLACEMENT_3D('',#17723,#14498,#14499);
#12159=AXIS2_PLACEMENT_3D('',#17725,#14501,#14502);
#12160=AXIS2_PLACEMENT_3D('',#17727,#14503,#14504);
#12161=AXIS2_PLACEMENT_3D('',#17729,#14506,#14507);
#12162=AXIS2_PLACEMENT_3D('',#17731,#14508,#14509);
#12163=AXIS2_PLACEMENT_3D('',#17733,#14511,#14512);
#12164=AXIS2_PLACEMENT_3D('',#17735,#14513,#14514);
#12165=AXIS2_PLACEMENT_3D('',#17737,#14516,#14517);
#12166=AXIS2_PLACEMENT_3D('',#17739,#14518,#14519);
#12167=AXIS2_PLACEMENT_3D('',#17741,#14521,#14522);
#12168=AXIS2_PLACEMENT_3D('',#17743,#14523,#14524);
#12169=AXIS2_PLACEMENT_3D('',#17745,#14526,#14527);
#12170=AXIS2_PLACEMENT_3D('',#17747,#14528,#14529);
#12171=AXIS2_PLACEMENT_3D('',#17749,#14531,#14532);
#12172=AXIS2_PLACEMENT_3D('',#17751,#14533,#14534);
#12173=AXIS2_PLACEMENT_3D('',#17753,#14536,#14537);
#12174=AXIS2_PLACEMENT_3D('',#17755,#14538,#14539);
#12175=AXIS2_PLACEMENT_3D('',#17757,#14541,#14542);
#12176=AXIS2_PLACEMENT_3D('',#17759,#14543,#14544);
#12177=AXIS2_PLACEMENT_3D('',#17761,#14546,#14547);
#12178=AXIS2_PLACEMENT_3D('',#17763,#14548,#14549);
#12179=AXIS2_PLACEMENT_3D('',#17765,#14551,#14552);
#12180=AXIS2_PLACEMENT_3D('',#17767,#14553,#14554);
#12181=AXIS2_PLACEMENT_3D('',#17769,#14556,#14557);
#12182=AXIS2_PLACEMENT_3D('',#17771,#14558,#14559);
#12183=AXIS2_PLACEMENT_3D('',#17773,#14561,#14562);
#12184=AXIS2_PLACEMENT_3D('',#17775,#14563,#14564);
#12185=AXIS2_PLACEMENT_3D('',#17777,#14566,#14567);
#12186=AXIS2_PLACEMENT_3D('',#17779,#14568,#14569);
#12187=AXIS2_PLACEMENT_3D('',#17781,#14571,#14572);
#12188=AXIS2_PLACEMENT_3D('',#17783,#14573,#14574);
#12189=AXIS2_PLACEMENT_3D('',#17785,#14576,#14577);
#12190=AXIS2_PLACEMENT_3D('',#17787,#14578,#14579);
#12191=AXIS2_PLACEMENT_3D('',#17789,#14581,#14582);
#12192=AXIS2_PLACEMENT_3D('',#17791,#14583,#14584);
#12193=AXIS2_PLACEMENT_3D('',#17793,#14586,#14587);
#12194=AXIS2_PLACEMENT_3D('',#17795,#14588,#14589);
#12195=AXIS2_PLACEMENT_3D('',#17797,#14591,#14592);
#12196=AXIS2_PLACEMENT_3D('',#17799,#14593,#14594);
#12197=AXIS2_PLACEMENT_3D('',#17801,#14596,#14597);
#12198=AXIS2_PLACEMENT_3D('',#17803,#14598,#14599);
#12199=AXIS2_PLACEMENT_3D('',#17805,#14601,#14602);
#12200=AXIS2_PLACEMENT_3D('',#17807,#14603,#14604);
#12201=AXIS2_PLACEMENT_3D('',#17809,#14606,#14607);
#12202=AXIS2_PLACEMENT_3D('',#17811,#14608,#14609);
#12203=AXIS2_PLACEMENT_3D('',#17813,#14611,#14612);
#12204=AXIS2_PLACEMENT_3D('',#17815,#14613,#14614);
#12205=AXIS2_PLACEMENT_3D('',#17817,#14616,#14617);
#12206=AXIS2_PLACEMENT_3D('',#17819,#14618,#14619);
#12207=AXIS2_PLACEMENT_3D('',#17821,#14621,#14622);
#12208=AXIS2_PLACEMENT_3D('',#17823,#14623,#14624);
#12209=AXIS2_PLACEMENT_3D('',#17825,#14626,#14627);
#12210=AXIS2_PLACEMENT_3D('',#17827,#14628,#14629);
#12211=AXIS2_PLACEMENT_3D('',#17829,#14631,#14632);
#12212=AXIS2_PLACEMENT_3D('',#17831,#14633,#14634);
#12213=AXIS2_PLACEMENT_3D('',#17833,#14636,#14637);
#12214=AXIS2_PLACEMENT_3D('',#17835,#14638,#14639);
#12215=AXIS2_PLACEMENT_3D('',#17837,#14641,#14642);
#12216=AXIS2_PLACEMENT_3D('',#17839,#14643,#14644);
#12217=AXIS2_PLACEMENT_3D('',#17841,#14646,#14647);
#12218=AXIS2_PLACEMENT_3D('',#17843,#14648,#14649);
#12219=AXIS2_PLACEMENT_3D('',#17845,#14651,#14652);
#12220=AXIS2_PLACEMENT_3D('',#17847,#14653,#14654);
#12221=AXIS2_PLACEMENT_3D('',#17849,#14656,#14657);
#12222=AXIS2_PLACEMENT_3D('',#17851,#14658,#14659);
#12223=AXIS2_PLACEMENT_3D('',#17853,#14661,#14662);
#12224=AXIS2_PLACEMENT_3D('',#17855,#14663,#14664);
#12225=AXIS2_PLACEMENT_3D('',#17857,#14666,#14667);
#12226=AXIS2_PLACEMENT_3D('',#17859,#14668,#14669);
#12227=AXIS2_PLACEMENT_3D('',#17861,#14671,#14672);
#12228=AXIS2_PLACEMENT_3D('',#17865,#14675,#14676);
#12229=AXIS2_PLACEMENT_3D('',#17867,#14678,#14679);
#12230=AXIS2_PLACEMENT_3D('',#17869,#14680,#14681);
#12231=AXIS2_PLACEMENT_3D('',#17872,#14683,#14684);
#12232=AXIS2_PLACEMENT_3D('',#17873,#14685,#14686);
#12233=AXIS2_PLACEMENT_3D('',#17875,#14687,#14688);
#12234=AXIS2_PLACEMENT_3D('',#17878,#14690,#14691);
#12235=AXIS2_PLACEMENT_3D('',#17879,#14692,#14693);
#12236=AXIS2_PLACEMENT_3D('',#17881,#14694,#14695);
#12237=AXIS2_PLACEMENT_3D('',#17884,#14697,#14698);
#12238=AXIS2_PLACEMENT_3D('',#17885,#14699,#14700);
#12239=AXIS2_PLACEMENT_3D('',#17887,#14701,#14702);
#12240=AXIS2_PLACEMENT_3D('',#17890,#14704,#14705);
#12241=AXIS2_PLACEMENT_3D('',#17891,#14706,#14707);
#12242=AXIS2_PLACEMENT_3D('',#17893,#14708,#14709);
#12243=AXIS2_PLACEMENT_3D('',#17896,#14711,#14712);
#12244=AXIS2_PLACEMENT_3D('',#17897,#14713,#14714);
#12245=AXIS2_PLACEMENT_3D('',#17899,#14715,#14716);
#12246=AXIS2_PLACEMENT_3D('',#17902,#14718,#14719);
#12247=AXIS2_PLACEMENT_3D('',#17903,#14720,#14721);
#12248=AXIS2_PLACEMENT_3D('',#17905,#14722,#14723);
#12249=AXIS2_PLACEMENT_3D('',#17908,#14725,#14726);
#12250=AXIS2_PLACEMENT_3D('',#17909,#14727,#14728);
#12251=AXIS2_PLACEMENT_3D('',#17911,#14729,#14730);
#12252=AXIS2_PLACEMENT_3D('',#17914,#14732,#14733);
#12253=AXIS2_PLACEMENT_3D('',#17915,#14734,#14735);
#12254=AXIS2_PLACEMENT_3D('',#17917,#14736,#14737);
#12255=AXIS2_PLACEMENT_3D('',#17920,#14739,#14740);
#12256=AXIS2_PLACEMENT_3D('',#17921,#14741,#14742);
#12257=AXIS2_PLACEMENT_3D('',#17923,#14743,#14744);
#12258=AXIS2_PLACEMENT_3D('',#17926,#14746,#14747);
#12259=AXIS2_PLACEMENT_3D('',#17927,#14748,#14749);
#12260=AXIS2_PLACEMENT_3D('',#17929,#14750,#14751);
#12261=AXIS2_PLACEMENT_3D('',#17932,#14753,#14754);
#12262=AXIS2_PLACEMENT_3D('',#17933,#14755,#14756);
#12263=AXIS2_PLACEMENT_3D('',#17935,#14757,#14758);
#12264=AXIS2_PLACEMENT_3D('',#17938,#14760,#14761);
#12265=AXIS2_PLACEMENT_3D('',#17939,#14762,#14763);
#12266=AXIS2_PLACEMENT_3D('',#17941,#14764,#14765);
#12267=AXIS2_PLACEMENT_3D('',#17944,#14767,#14768);
#12268=AXIS2_PLACEMENT_3D('',#17945,#14769,#14770);
#12269=AXIS2_PLACEMENT_3D('',#17947,#14771,#14772);
#12270=AXIS2_PLACEMENT_3D('',#17950,#14774,#14775);
#12271=AXIS2_PLACEMENT_3D('',#17951,#14776,#14777);
#12272=AXIS2_PLACEMENT_3D('',#17953,#14778,#14779);
#12273=AXIS2_PLACEMENT_3D('',#17956,#14781,#14782);
#12274=AXIS2_PLACEMENT_3D('',#17957,#14783,#14784);
#12275=AXIS2_PLACEMENT_3D('',#17959,#14785,#14786);
#12276=AXIS2_PLACEMENT_3D('',#17962,#14788,#14789);
#12277=AXIS2_PLACEMENT_3D('',#17963,#14790,#14791);
#12278=AXIS2_PLACEMENT_3D('',#17965,#14792,#14793);
#12279=AXIS2_PLACEMENT_3D('',#17968,#14795,#14796);
#12280=AXIS2_PLACEMENT_3D('',#17969,#14797,#14798);
#12281=AXIS2_PLACEMENT_3D('',#17971,#14799,#14800);
#12282=AXIS2_PLACEMENT_3D('',#17974,#14802,#14803);
#12283=AXIS2_PLACEMENT_3D('',#17975,#14804,#14805);
#12284=AXIS2_PLACEMENT_3D('',#17977,#14806,#14807);
#12285=AXIS2_PLACEMENT_3D('',#17980,#14809,#14810);
#12286=AXIS2_PLACEMENT_3D('',#17981,#14811,#14812);
#12287=AXIS2_PLACEMENT_3D('',#17983,#14813,#14814);
#12288=AXIS2_PLACEMENT_3D('',#17986,#14816,#14817);
#12289=AXIS2_PLACEMENT_3D('',#17987,#14818,#14819);
#12290=AXIS2_PLACEMENT_3D('',#17989,#14820,#14821);
#12291=AXIS2_PLACEMENT_3D('',#17992,#14823,#14824);
#12292=AXIS2_PLACEMENT_3D('',#17993,#14825,#14826);
#12293=AXIS2_PLACEMENT_3D('',#17995,#14827,#14828);
#12294=AXIS2_PLACEMENT_3D('',#17998,#14830,#14831);
#12295=AXIS2_PLACEMENT_3D('',#17999,#14832,#14833);
#12296=AXIS2_PLACEMENT_3D('',#18001,#14834,#14835);
#12297=AXIS2_PLACEMENT_3D('',#18004,#14837,#14838);
#12298=AXIS2_PLACEMENT_3D('',#18005,#14839,#14840);
#12299=AXIS2_PLACEMENT_3D('',#18007,#14841,#14842);
#12300=AXIS2_PLACEMENT_3D('',#18010,#14844,#14845);
#12301=AXIS2_PLACEMENT_3D('',#18011,#14846,#14847);
#12302=AXIS2_PLACEMENT_3D('',#18013,#14848,#14849);
#12303=AXIS2_PLACEMENT_3D('',#18016,#14851,#14852);
#12304=AXIS2_PLACEMENT_3D('',#18017,#14853,#14854);
#12305=AXIS2_PLACEMENT_3D('',#18019,#14855,#14856);
#12306=AXIS2_PLACEMENT_3D('',#18022,#14858,#14859);
#12307=AXIS2_PLACEMENT_3D('',#18023,#14860,#14861);
#12308=AXIS2_PLACEMENT_3D('',#18025,#14862,#14863);
#12309=AXIS2_PLACEMENT_3D('',#18028,#14865,#14866);
#12310=AXIS2_PLACEMENT_3D('',#18029,#14867,#14868);
#12311=AXIS2_PLACEMENT_3D('',#18031,#14869,#14870);
#12312=AXIS2_PLACEMENT_3D('',#18034,#14872,#14873);
#12313=AXIS2_PLACEMENT_3D('',#18035,#14874,#14875);
#12314=AXIS2_PLACEMENT_3D('',#18037,#14876,#14877);
#12315=AXIS2_PLACEMENT_3D('',#18040,#14879,#14880);
#12316=AXIS2_PLACEMENT_3D('',#18041,#14881,#14882);
#12317=AXIS2_PLACEMENT_3D('',#18043,#14883,#14884);
#12318=AXIS2_PLACEMENT_3D('',#18046,#14886,#14887);
#12319=AXIS2_PLACEMENT_3D('',#18047,#14888,#14889);
#12320=AXIS2_PLACEMENT_3D('',#18049,#14890,#14891);
#12321=AXIS2_PLACEMENT_3D('',#18052,#14893,#14894);
#12322=AXIS2_PLACEMENT_3D('',#18053,#14895,#14896);
#12323=AXIS2_PLACEMENT_3D('',#18055,#14897,#14898);
#12324=AXIS2_PLACEMENT_3D('',#18058,#14900,#14901);
#12325=AXIS2_PLACEMENT_3D('',#18059,#14902,#14903);
#12326=AXIS2_PLACEMENT_3D('',#18061,#14904,#14905);
#12327=AXIS2_PLACEMENT_3D('',#18064,#14907,#14908);
#12328=AXIS2_PLACEMENT_3D('',#18065,#14909,#14910);
#12329=AXIS2_PLACEMENT_3D('',#18067,#14911,#14912);
#12330=AXIS2_PLACEMENT_3D('',#18070,#14914,#14915);
#12331=AXIS2_PLACEMENT_3D('',#18071,#14916,#14917);
#12332=AXIS2_PLACEMENT_3D('',#18073,#14918,#14919);
#12333=AXIS2_PLACEMENT_3D('',#18076,#14921,#14922);
#12334=AXIS2_PLACEMENT_3D('',#18077,#14923,#14924);
#12335=AXIS2_PLACEMENT_3D('',#18079,#14925,#14926);
#12336=AXIS2_PLACEMENT_3D('',#18082,#14928,#14929);
#12337=AXIS2_PLACEMENT_3D('',#18083,#14930,#14931);
#12338=AXIS2_PLACEMENT_3D('',#18085,#14932,#14933);
#12339=AXIS2_PLACEMENT_3D('',#18088,#14935,#14936);
#12340=AXIS2_PLACEMENT_3D('',#18089,#14937,#14938);
#12341=AXIS2_PLACEMENT_3D('',#18091,#14939,#14940);
#12342=AXIS2_PLACEMENT_3D('',#18094,#14942,#14943);
#12343=AXIS2_PLACEMENT_3D('',#18095,#14944,#14945);
#12344=AXIS2_PLACEMENT_3D('',#18097,#14946,#14947);
#12345=AXIS2_PLACEMENT_3D('',#18100,#14949,#14950);
#12346=AXIS2_PLACEMENT_3D('',#18101,#14951,#14952);
#12347=AXIS2_PLACEMENT_3D('',#18103,#14953,#14954);
#12348=AXIS2_PLACEMENT_3D('',#18106,#14956,#14957);
#12349=AXIS2_PLACEMENT_3D('',#18107,#14958,#14959);
#12350=AXIS2_PLACEMENT_3D('',#18109,#14960,#14961);
#12351=AXIS2_PLACEMENT_3D('',#18112,#14963,#14964);
#12352=AXIS2_PLACEMENT_3D('',#18113,#14965,#14966);
#12353=AXIS2_PLACEMENT_3D('',#18115,#14967,#14968);
#12354=AXIS2_PLACEMENT_3D('',#18118,#14970,#14971);
#12355=AXIS2_PLACEMENT_3D('',#18119,#14972,#14973);
#12356=AXIS2_PLACEMENT_3D('',#18121,#14974,#14975);
#12357=AXIS2_PLACEMENT_3D('',#18124,#14977,#14978);
#12358=AXIS2_PLACEMENT_3D('',#18125,#14979,#14980);
#12359=AXIS2_PLACEMENT_3D('',#18127,#14981,#14982);
#12360=AXIS2_PLACEMENT_3D('',#18130,#14984,#14985);
#12361=AXIS2_PLACEMENT_3D('',#18131,#14986,#14987);
#12362=AXIS2_PLACEMENT_3D('',#18133,#14988,#14989);
#12363=AXIS2_PLACEMENT_3D('',#18136,#14991,#14992);
#12364=AXIS2_PLACEMENT_3D('',#18137,#14993,#14994);
#12365=AXIS2_PLACEMENT_3D('',#18139,#14995,#14996);
#12366=AXIS2_PLACEMENT_3D('',#18142,#14998,#14999);
#12367=AXIS2_PLACEMENT_3D('',#18143,#15000,#15001);
#12368=AXIS2_PLACEMENT_3D('',#18145,#15002,#15003);
#12369=AXIS2_PLACEMENT_3D('',#18148,#15005,#15006);
#12370=AXIS2_PLACEMENT_3D('',#18149,#15007,#15008);
#12371=AXIS2_PLACEMENT_3D('',#18155,#15012,#15013);
#12372=AXIS2_PLACEMENT_3D('',#18158,#15016,#15017);
#12373=AXIS2_PLACEMENT_3D('',#18159,#15018,#15019);
#12374=AXIS2_PLACEMENT_3D('',#18160,#15020,#15021);
#12375=AXIS2_PLACEMENT_3D('',#18161,#15022,#15023);
#12376=AXIS2_PLACEMENT_3D('',#18163,#15024,#15025);
#12377=AXIS2_PLACEMENT_3D('',#18166,#15027,#15028);
#12378=AXIS2_PLACEMENT_3D('',#18167,#15029,#15030);
#12379=AXIS2_PLACEMENT_3D('',#18169,#15031,#15032);
#12380=AXIS2_PLACEMENT_3D('',#18172,#15034,#15035);
#12381=AXIS2_PLACEMENT_3D('',#18173,#15036,#15037);
#12382=AXIS2_PLACEMENT_3D('',#18175,#15038,#15039);
#12383=AXIS2_PLACEMENT_3D('',#18178,#15041,#15042);
#12384=AXIS2_PLACEMENT_3D('',#18179,#15043,#15044);
#12385=AXIS2_PLACEMENT_3D('',#18182,#15045,#15046);
#12386=AXIS2_PLACEMENT_3D('',#18186,#15048,#15049);
#12387=AXIS2_PLACEMENT_3D('',#18188,#15051,#15052);
#12388=AXIS2_PLACEMENT_3D('',#18203,#15060,#15061);
#12389=AXIS2_PLACEMENT_3D('',#18205,#15062,#15063);
#12390=AXIS2_PLACEMENT_3D('',#18207,#15064,#15065);
#12391=AXIS2_PLACEMENT_3D('',#18209,#15066,#15067);
#12392=AXIS2_PLACEMENT_3D('',#18211,#15068,#15069);
#12393=AXIS2_PLACEMENT_3D('',#18213,#15070,#15071);
#12394=AXIS2_PLACEMENT_3D('',#18215,#15072,#15073);
#12395=AXIS2_PLACEMENT_3D('',#18217,#15074,#15075);
#12396=AXIS2_PLACEMENT_3D('',#18219,#15076,#15077);
#12397=AXIS2_PLACEMENT_3D('',#18221,#15078,#15079);
#12398=AXIS2_PLACEMENT_3D('',#18223,#15080,#15081);
#12399=AXIS2_PLACEMENT_3D('',#18224,#15082,#15083);
#12400=AXIS2_PLACEMENT_3D('',#18227,#15084,#15085);
#12401=AXIS2_PLACEMENT_3D('',#18231,#15087,#15088);
#12402=AXIS2_PLACEMENT_3D('',#18233,#15090,#15091);
#12403=AXIS2_PLACEMENT_3D('',#18248,#15099,#15100);
#12404=AXIS2_PLACEMENT_3D('',#18250,#15101,#15102);
#12405=AXIS2_PLACEMENT_3D('',#18252,#15103,#15104);
#12406=AXIS2_PLACEMENT_3D('',#18254,#15105,#15106);
#12407=AXIS2_PLACEMENT_3D('',#18256,#15107,#15108);
#12408=AXIS2_PLACEMENT_3D('',#18258,#15109,#15110);
#12409=AXIS2_PLACEMENT_3D('',#18260,#15111,#15112);
#12410=AXIS2_PLACEMENT_3D('',#18262,#15113,#15114);
#12411=AXIS2_PLACEMENT_3D('',#18264,#15115,#15116);
#12412=AXIS2_PLACEMENT_3D('',#18266,#15117,#15118);
#12413=AXIS2_PLACEMENT_3D('',#18268,#15119,#15120);
#12414=AXIS2_PLACEMENT_3D('',#18269,#15121,#15122);
#12415=AXIS2_PLACEMENT_3D('',#18271,#15124,#15125);
#12416=AXIS2_PLACEMENT_3D('',#18273,#15127,#15128);
#12417=AXIS2_PLACEMENT_3D('',#18275,#15130,#15131);
#12418=AXIS2_PLACEMENT_3D('',#18277,#15133,#15134);
#12419=AXIS2_PLACEMENT_3D('',#18279,#15136,#15137);
#12420=AXIS2_PLACEMENT_3D('',#18281,#15139,#15140);
#12421=AXIS2_PLACEMENT_3D('',#18283,#15142,#15143);
#12422=AXIS2_PLACEMENT_3D('',#18285,#15145,#15146);
#12423=AXIS2_PLACEMENT_3D('',#18287,#15148,#15149);
#12424=AXIS2_PLACEMENT_3D('',#18289,#15151,#15152);
#12425=AXIS2_PLACEMENT_3D('',#18291,#15154,#15155);
#12426=AXIS2_PLACEMENT_3D('',#18294,#15158,#15159);
#12427=AXIS2_PLACEMENT_3D('',#18297,#15162,#15163);
#12428=AXIS2_PLACEMENT_3D('',#18299,#15165,#15166);
#12429=AXIS2_PLACEMENT_3D('',#18301,#15168,#15169);
#12430=AXIS2_PLACEMENT_3D('',#18302,#15170,#15171);
#12431=AXIS2_PLACEMENT_3D('',#18320,#15180,#15181);
#12432=AXIS2_PLACEMENT_3D('',#18322,#15182,#15183);
#12433=AXIS2_PLACEMENT_3D('',#18324,#15184,#15185);
#12434=AXIS2_PLACEMENT_3D('',#18326,#15186,#15187);
#12435=AXIS2_PLACEMENT_3D('',#18328,#15188,#15189);
#12436=AXIS2_PLACEMENT_3D('',#18330,#15190,#15191);
#12437=AXIS2_PLACEMENT_3D('',#18332,#15192,#15193);
#12438=AXIS2_PLACEMENT_3D('',#18334,#15194,#15195);
#12439=AXIS2_PLACEMENT_3D('',#18336,#15196,#15197);
#12440=AXIS2_PLACEMENT_3D('',#18338,#15198,#15199);
#12441=AXIS2_PLACEMENT_3D('',#18340,#15200,#15201);
#12442=AXIS2_PLACEMENT_3D('',#18341,#15202,#15203);
#12443=AXIS2_PLACEMENT_3D('',#18343,#15204,#15205);
#12444=AXIS2_PLACEMENT_3D('',#18345,#15207,#15208);
#12445=AXIS2_PLACEMENT_3D('',#18347,#15209,#15210);
#12446=AXIS2_PLACEMENT_3D('',#18349,#15212,#15213);
#12447=AXIS2_PLACEMENT_3D('',#18351,#15214,#15215);
#12448=AXIS2_PLACEMENT_3D('',#18353,#15217,#15218);
#12449=AXIS2_PLACEMENT_3D('',#18355,#15219,#15220);
#12450=AXIS2_PLACEMENT_3D('',#18357,#15222,#15223);
#12451=AXIS2_PLACEMENT_3D('',#18359,#15224,#15225);
#12452=AXIS2_PLACEMENT_3D('',#18361,#15227,#15228);
#12453=AXIS2_PLACEMENT_3D('',#18363,#15229,#15230);
#12454=AXIS2_PLACEMENT_3D('',#18365,#15232,#15233);
#12455=AXIS2_PLACEMENT_3D('',#18367,#15234,#15235);
#12456=AXIS2_PLACEMENT_3D('',#18369,#15237,#15238);
#12457=AXIS2_PLACEMENT_3D('',#18371,#15239,#15240);
#12458=AXIS2_PLACEMENT_3D('',#18373,#15242,#15243);
#12459=AXIS2_PLACEMENT_3D('',#18375,#15244,#15245);
#12460=AXIS2_PLACEMENT_3D('',#18377,#15247,#15248);
#12461=AXIS2_PLACEMENT_3D('',#18379,#15249,#15250);
#12462=AXIS2_PLACEMENT_3D('',#18381,#15252,#15253);
#12463=AXIS2_PLACEMENT_3D('',#18383,#15254,#15255);
#12464=AXIS2_PLACEMENT_3D('',#18385,#15257,#15258);
#12465=AXIS2_PLACEMENT_3D('',#18391,#15262,#15263);
#12466=AXIS2_PLACEMENT_3D('',#18397,#15267,#15268);
#12467=AXIS2_PLACEMENT_3D('',#18401,#15271,#15272);
#12468=AXIS2_PLACEMENT_3D('',#18405,#15275,#15276);
#12469=AXIS2_PLACEMENT_3D('',#18407,#15278,#15279);
#12470=AXIS2_PLACEMENT_3D('',#18413,#15283,#15284);
#12471=AXIS2_PLACEMENT_3D('',#18419,#15288,#15289);
#12472=AXIS2_PLACEMENT_3D('',#18422,#15292,#15293);
#12473=AXIS2_PLACEMENT_3D('',#18426,#15296,#15297);
#12474=AXIS2_PLACEMENT_3D('',#18430,#15300,#15301);
#12475=AXIS2_PLACEMENT_3D('',#18432,#15303,#15304);
#12476=AXIS2_PLACEMENT_3D('',#18433,#15305,#15306);
#12477=AXIS2_PLACEMENT_3D('',#18434,#15307,#15308);
#12478=AXIS2_PLACEMENT_3D('',#18436,#15309,#15310);
#12479=AXIS2_PLACEMENT_3D('',#18439,#15312,#15313);
#12480=AXIS2_PLACEMENT_3D('',#18440,#15314,#15315);
#12481=AXIS2_PLACEMENT_3D('',#18449,#15320,#15321);
#12482=AXIS2_PLACEMENT_3D('',#18455,#15325,#15326);
#12483=AXIS2_PLACEMENT_3D('',#18461,#15330,#15331);
#12484=AXIS2_PLACEMENT_3D('',#18467,#15335,#15336);
#12485=AXIS2_PLACEMENT_3D('',#18473,#15340,#15341);
#12486=AXIS2_PLACEMENT_3D('',#18476,#15344,#15345);
#12487=AXIS2_PLACEMENT_3D('',#18477,#15346,#15347);
#12488=AXIS2_PLACEMENT_3D('',#18478,#15348,#15349);
#12489=AXIS2_PLACEMENT_3D('',#18479,#15350,#15351);
#12490=AXIS2_PLACEMENT_3D('',#18481,#15352,#15353);
#12491=AXIS2_PLACEMENT_3D('',#18484,#15355,#15356);
#12492=AXIS2_PLACEMENT_3D('',#18485,#15357,#15358);
#12493=AXIS2_PLACEMENT_3D('',#18487,#15359,#15360);
#12494=AXIS2_PLACEMENT_3D('',#18490,#15362,#15363);
#12495=AXIS2_PLACEMENT_3D('',#18491,#15364,#15365);
#12496=AXIS2_PLACEMENT_3D('',#18493,#15366,#15367);
#12497=AXIS2_PLACEMENT_3D('',#18496,#15369,#15370);
#12498=AXIS2_PLACEMENT_3D('',#18497,#15371,#15372);
#12499=AXIS2_PLACEMENT_3D('',#18500,#15373,#15374);
#12500=AXIS2_PLACEMENT_3D('',#18504,#15376,#15377);
#12501=AXIS2_PLACEMENT_3D('',#18506,#15379,#15380);
#12502=AXIS2_PLACEMENT_3D('',#18521,#15388,#15389);
#12503=AXIS2_PLACEMENT_3D('',#18523,#15390,#15391);
#12504=AXIS2_PLACEMENT_3D('',#18525,#15392,#15393);
#12505=AXIS2_PLACEMENT_3D('',#18527,#15394,#15395);
#12506=AXIS2_PLACEMENT_3D('',#18529,#15396,#15397);
#12507=AXIS2_PLACEMENT_3D('',#18531,#15398,#15399);
#12508=AXIS2_PLACEMENT_3D('',#18533,#15400,#15401);
#12509=AXIS2_PLACEMENT_3D('',#18535,#15402,#15403);
#12510=AXIS2_PLACEMENT_3D('',#18537,#15404,#15405);
#12511=AXIS2_PLACEMENT_3D('',#18539,#15406,#15407);
#12512=AXIS2_PLACEMENT_3D('',#18541,#15408,#15409);
#12513=AXIS2_PLACEMENT_3D('',#18542,#15410,#15411);
#12514=AXIS2_PLACEMENT_3D('',#18545,#15412,#15413);
#12515=AXIS2_PLACEMENT_3D('',#18549,#15415,#15416);
#12516=AXIS2_PLACEMENT_3D('',#18551,#15418,#15419);
#12517=AXIS2_PLACEMENT_3D('',#18566,#15427,#15428);
#12518=AXIS2_PLACEMENT_3D('',#18568,#15429,#15430);
#12519=AXIS2_PLACEMENT_3D('',#18570,#15431,#15432);
#12520=AXIS2_PLACEMENT_3D('',#18572,#15433,#15434);
#12521=AXIS2_PLACEMENT_3D('',#18574,#15435,#15436);
#12522=AXIS2_PLACEMENT_3D('',#18576,#15437,#15438);
#12523=AXIS2_PLACEMENT_3D('',#18578,#15439,#15440);
#12524=AXIS2_PLACEMENT_3D('',#18580,#15441,#15442);
#12525=AXIS2_PLACEMENT_3D('',#18582,#15443,#15444);
#12526=AXIS2_PLACEMENT_3D('',#18584,#15445,#15446);
#12527=AXIS2_PLACEMENT_3D('',#18586,#15447,#15448);
#12528=AXIS2_PLACEMENT_3D('',#18587,#15449,#15450);
#12529=AXIS2_PLACEMENT_3D('',#18589,#15452,#15453);
#12530=AXIS2_PLACEMENT_3D('',#18591,#15455,#15456);
#12531=AXIS2_PLACEMENT_3D('',#18593,#15458,#15459);
#12532=AXIS2_PLACEMENT_3D('',#18595,#15461,#15462);
#12533=AXIS2_PLACEMENT_3D('',#18597,#15464,#15465);
#12534=AXIS2_PLACEMENT_3D('',#18599,#15467,#15468);
#12535=AXIS2_PLACEMENT_3D('',#18601,#15470,#15471);
#12536=AXIS2_PLACEMENT_3D('',#18603,#15473,#15474);
#12537=AXIS2_PLACEMENT_3D('',#18605,#15476,#15477);
#12538=AXIS2_PLACEMENT_3D('',#18607,#15479,#15480);
#12539=AXIS2_PLACEMENT_3D('',#18609,#15482,#15483);
#12540=AXIS2_PLACEMENT_3D('',#18612,#15486,#15487);
#12541=AXIS2_PLACEMENT_3D('',#18615,#15490,#15491);
#12542=AXIS2_PLACEMENT_3D('',#18617,#15493,#15494);
#12543=AXIS2_PLACEMENT_3D('',#18619,#15496,#15497);
#12544=AXIS2_PLACEMENT_3D('',#18620,#15498,#15499);
#12545=AXIS2_PLACEMENT_3D('',#18638,#15508,#15509);
#12546=AXIS2_PLACEMENT_3D('',#18640,#15510,#15511);
#12547=AXIS2_PLACEMENT_3D('',#18642,#15512,#15513);
#12548=AXIS2_PLACEMENT_3D('',#18644,#15514,#15515);
#12549=AXIS2_PLACEMENT_3D('',#18646,#15516,#15517);
#12550=AXIS2_PLACEMENT_3D('',#18648,#15518,#15519);
#12551=AXIS2_PLACEMENT_3D('',#18650,#15520,#15521);
#12552=AXIS2_PLACEMENT_3D('',#18652,#15522,#15523);
#12553=AXIS2_PLACEMENT_3D('',#18654,#15524,#15525);
#12554=AXIS2_PLACEMENT_3D('',#18656,#15526,#15527);
#12555=AXIS2_PLACEMENT_3D('',#18658,#15528,#15529);
#12556=AXIS2_PLACEMENT_3D('',#18659,#15530,#15531);
#12557=AXIS2_PLACEMENT_3D('',#18661,#15532,#15533);
#12558=AXIS2_PLACEMENT_3D('',#18663,#15535,#15536);
#12559=AXIS2_PLACEMENT_3D('',#18665,#15537,#15538);
#12560=AXIS2_PLACEMENT_3D('',#18667,#15540,#15541);
#12561=AXIS2_PLACEMENT_3D('',#18669,#15542,#15543);
#12562=AXIS2_PLACEMENT_3D('',#18671,#15545,#15546);
#12563=AXIS2_PLACEMENT_3D('',#18673,#15547,#15548);
#12564=AXIS2_PLACEMENT_3D('',#18675,#15550,#15551);
#12565=AXIS2_PLACEMENT_3D('',#18677,#15552,#15553);
#12566=AXIS2_PLACEMENT_3D('',#18679,#15555,#15556);
#12567=AXIS2_PLACEMENT_3D('',#18681,#15557,#15558);
#12568=AXIS2_PLACEMENT_3D('',#18683,#15560,#15561);
#12569=AXIS2_PLACEMENT_3D('',#18685,#15562,#15563);
#12570=AXIS2_PLACEMENT_3D('',#18687,#15565,#15566);
#12571=AXIS2_PLACEMENT_3D('',#18689,#15567,#15568);
#12572=AXIS2_PLACEMENT_3D('',#18691,#15570,#15571);
#12573=AXIS2_PLACEMENT_3D('',#18693,#15572,#15573);
#12574=AXIS2_PLACEMENT_3D('',#18695,#15575,#15576);
#12575=AXIS2_PLACEMENT_3D('',#18697,#15577,#15578);
#12576=AXIS2_PLACEMENT_3D('',#18699,#15580,#15581);
#12577=AXIS2_PLACEMENT_3D('',#18701,#15582,#15583);
#12578=AXIS2_PLACEMENT_3D('',#18703,#15585,#15586);
#12579=AXIS2_PLACEMENT_3D('',#18709,#15590,#15591);
#12580=AXIS2_PLACEMENT_3D('',#18715,#15595,#15596);
#12581=AXIS2_PLACEMENT_3D('',#18719,#15599,#15600);
#12582=AXIS2_PLACEMENT_3D('',#18723,#15603,#15604);
#12583=AXIS2_PLACEMENT_3D('',#18725,#15606,#15607);
#12584=AXIS2_PLACEMENT_3D('',#18731,#15611,#15612);
#12585=AXIS2_PLACEMENT_3D('',#18737,#15616,#15617);
#12586=AXIS2_PLACEMENT_3D('',#18740,#15620,#15621);
#12587=AXIS2_PLACEMENT_3D('',#18744,#15624,#15625);
#12588=AXIS2_PLACEMENT_3D('',#18748,#15628,#15629);
#12589=AXIS2_PLACEMENT_3D('',#18750,#15631,#15632);
#12590=AXIS2_PLACEMENT_3D('',#18751,#15633,#15634);
#12591=AXIS2_PLACEMENT_3D('',#18752,#15635,#15636);
#12592=AXIS2_PLACEMENT_3D('',#18766,#15643,#15644);
#12593=AXIS2_PLACEMENT_3D('',#18767,#15645,#15646);
#12594=AXIS2_PLACEMENT_3D('',#18773,#15650,#15651);
#12595=AXIS2_PLACEMENT_3D('',#18777,#15654,#15655);
#12596=AXIS2_PLACEMENT_3D('',#18781,#15658,#15659);
#12597=AXIS2_PLACEMENT_3D('',#18785,#15662,#15663);
#12598=AXIS2_PLACEMENT_3D('',#18789,#15666,#15667);
#12599=AXIS2_PLACEMENT_3D('',#18791,#15669,#15670);
#12600=AXIS2_PLACEMENT_3D('',#18792,#15671,#15672);
#12601=AXIS2_PLACEMENT_3D('',#18794,#15673,#15674);
#12602=AXIS2_PLACEMENT_3D('',#18796,#15676,#15677);
#12603=AXIS2_PLACEMENT_3D('',#18797,#15678,#15679);
#12604=AXIS2_PLACEMENT_3D('',#18798,#15680,#15681);
#12605=AXIS2_PLACEMENT_3D('',#18800,#15682,#15683);
#12606=AXIS2_PLACEMENT_3D('',#18803,#15685,#15686);
#12607=AXIS2_PLACEMENT_3D('',#18804,#15687,#15688);
#12608=AXIS2_PLACEMENT_3D('',#18813,#15693,#15694);
#12609=AXIS2_PLACEMENT_3D('',#18819,#15698,#15699);
#12610=AXIS2_PLACEMENT_3D('',#18825,#15703,#15704);
#12611=AXIS2_PLACEMENT_3D('',#18831,#15708,#15709);
#12612=AXIS2_PLACEMENT_3D('',#18837,#15713,#15714);
#12613=AXIS2_PLACEMENT_3D('',#18840,#15717,#15718);
#12614=AXIS2_PLACEMENT_3D('',#18841,#15719,#15720);
#12615=AXIS2_PLACEMENT_3D('',#18842,#15721,#15722);
#12616=AXIS2_PLACEMENT_3D('',#18843,#15723,#15724);
#12617=AXIS2_PLACEMENT_3D('',#18845,#15725,#15726);
#12618=AXIS2_PLACEMENT_3D('',#18848,#15728,#15729);
#12619=AXIS2_PLACEMENT_3D('',#18849,#15730,#15731);
#12620=AXIS2_PLACEMENT_3D('',#18858,#15736,#15737);
#12621=AXIS2_PLACEMENT_3D('',#18864,#15741,#15742);
#12622=AXIS2_PLACEMENT_3D('',#18870,#15746,#15747);
#12623=AXIS2_PLACEMENT_3D('',#18876,#15751,#15752);
#12624=AXIS2_PLACEMENT_3D('',#18882,#15756,#15757);
#12625=AXIS2_PLACEMENT_3D('',#18885,#15760,#15761);
#12626=AXIS2_PLACEMENT_3D('',#18886,#15762,#15763);
#12627=AXIS2_PLACEMENT_3D('',#18887,#15764,#15765);
#12628=AXIS2_PLACEMENT_3D('',#18888,#15766,#15767);
#12629=AXIS2_PLACEMENT_3D('',#18897,#15772,#15773);
#12630=AXIS2_PLACEMENT_3D('',#18899,#15774,#15775);
#12631=AXIS2_PLACEMENT_3D('',#18902,#15777,#15778);
#12632=AXIS2_PLACEMENT_3D('',#18903,#15779,#15780);
#12633=AXIS2_PLACEMENT_3D('',#18909,#15784,#15785);
#12634=AXIS2_PLACEMENT_3D('',#18918,#15790,#15791);
#12635=AXIS2_PLACEMENT_3D('',#18920,#15792,#15793);
#12636=AXIS2_PLACEMENT_3D('',#18923,#15795,#15796);
#12637=AXIS2_PLACEMENT_3D('',#18924,#15797,#15798);
#12638=AXIS2_PLACEMENT_3D('',#18930,#15802,#15803);
#12639=AXIS2_PLACEMENT_3D('',#18932,#15804,#15805);
#12640=AXIS2_PLACEMENT_3D('',#18935,#15807,#15808);
#12641=AXIS2_PLACEMENT_3D('',#18936,#15809,#15810);
#12642=AXIS2_PLACEMENT_3D('',#18938,#15811,#15812);
#12643=AXIS2_PLACEMENT_3D('',#18940,#15813,#15814);
#12644=AXIS2_PLACEMENT_3D('',#18942,#15816,#15817);
#12645=AXIS2_PLACEMENT_3D('',#18948,#15821,#15822);
#12646=AXIS2_PLACEMENT_3D('',#18957,#15827,#15828);
#12647=AXIS2_PLACEMENT_3D('',#18959,#15829,#15830);
#12648=AXIS2_PLACEMENT_3D('',#18961,#15831,#15832);
#12649=AXIS2_PLACEMENT_3D('',#18963,#15834,#15835);
#12650=AXIS2_PLACEMENT_3D('',#18969,#15839,#15840);
#12651=AXIS2_PLACEMENT_3D('',#18978,#15845,#15846);
#12652=AXIS2_PLACEMENT_3D('',#18980,#15847,#15848);
#12653=AXIS2_PLACEMENT_3D('',#18982,#15849,#15850);
#12654=AXIS2_PLACEMENT_3D('',#18984,#15852,#15853);
#12655=AXIS2_PLACEMENT_3D('',#18990,#15857,#15858);
#12656=AXIS2_PLACEMENT_3D('',#18991,#15859,#15860);
#12657=AXIS2_PLACEMENT_3D('',#18992,#15861,#15862);
#12658=AXIS2_PLACEMENT_3D('',#18993,#15863,#15864);
#12659=AXIS2_PLACEMENT_3D('',#18999,#15868,#15869);
#12660=AXIS2_PLACEMENT_3D('',#19000,#15870,#15871);
#12661=AXIS2_PLACEMENT_3D('',#19001,#15872,#15873);
#12662=AXIS2_PLACEMENT_3D('',#19002,#15874,#15875);
#12663=AXIS2_PLACEMENT_3D('',#19008,#15879,#15880);
#12664=AXIS2_PLACEMENT_3D('',#19014,#15884,#15885);
#12665=AXIS2_PLACEMENT_3D('',#19017,#15888,#15889);
#12666=AXIS2_PLACEMENT_3D('',#19019,#15890,#15891);
#12667=AXIS2_PLACEMENT_3D('',#19022,#15893,#15894);
#12668=AXIS2_PLACEMENT_3D('',#19023,#15895,#15896);
#12669=AXIS2_PLACEMENT_3D('',#19029,#15900,#15901);
#12670=AXIS2_PLACEMENT_3D('',#19031,#15902,#15903);
#12671=AXIS2_PLACEMENT_3D('',#19034,#15905,#15906);
#12672=AXIS2_PLACEMENT_3D('',#19035,#15907,#15908);
#12673=AXIS2_PLACEMENT_3D('',#19041,#15912,#15913);
#12674=AXIS2_PLACEMENT_3D('',#19047,#15917,#15918);
#12675=AXIS2_PLACEMENT_3D('',#19053,#15922,#15923);
#12676=AXIS2_PLACEMENT_3D('',#19055,#15924,#15925);
#12677=AXIS2_PLACEMENT_3D('',#19058,#15927,#15928);
#12678=AXIS2_PLACEMENT_3D('',#19059,#15929,#15930);
#12679=AXIS2_PLACEMENT_3D('',#19065,#15934,#15935);
#12680=AXIS2_PLACEMENT_3D('',#19067,#15936,#15937);
#12681=AXIS2_PLACEMENT_3D('',#19070,#15939,#15940);
#12682=AXIS2_PLACEMENT_3D('',#19071,#15941,#15942);
#12683=AXIS2_PLACEMENT_3D('',#19077,#15946,#15947);
#12684=AXIS2_PLACEMENT_3D('',#19079,#15948,#15949);
#12685=AXIS2_PLACEMENT_3D('',#19081,#15950,#15951);
#12686=AXIS2_PLACEMENT_3D('',#19083,#15953,#15954);
#12687=AXIS2_PLACEMENT_3D('',#19089,#15958,#15959);
#12688=AXIS2_PLACEMENT_3D('',#19091,#15960,#15961);
#12689=AXIS2_PLACEMENT_3D('',#19093,#15962,#15963);
#12690=AXIS2_PLACEMENT_3D('',#19095,#15965,#15966);
#12691=AXIS2_PLACEMENT_3D('',#19101,#15970,#15971);
#12692=AXIS2_PLACEMENT_3D('',#19107,#15975,#15976);
#12693=AXIS2_PLACEMENT_3D('',#19113,#15980,#15981);
#12694=AXIS2_PLACEMENT_3D('',#19115,#15982,#15983);
#12695=AXIS2_PLACEMENT_3D('',#19117,#15984,#15985);
#12696=AXIS2_PLACEMENT_3D('',#19119,#15987,#15988);
#12697=AXIS2_PLACEMENT_3D('',#19125,#15992,#15993);
#12698=AXIS2_PLACEMENT_3D('',#19126,#15994,#15995);
#12699=AXIS2_PLACEMENT_3D('',#19127,#15996,#15997);
#12700=AXIS2_PLACEMENT_3D('',#19128,#15998,#15999);
#12701=AXIS2_PLACEMENT_3D('',#19129,#16000,#16001);
#12702=AXIS2_PLACEMENT_3D('',#19130,#16002,#16003);
#12703=AXIS2_PLACEMENT_3D('',#19131,#16004,#16005);
#12704=AXIS2_PLACEMENT_3D('',#19133,#16006,#16007);
#12705=AXIS2_PLACEMENT_3D('',#19136,#16009,#16010);
#12706=AXIS2_PLACEMENT_3D('',#19137,#16011,#16012);
#12707=AXIS2_PLACEMENT_3D('',#19146,#16017,#16018);
#12708=AXIS2_PLACEMENT_3D('',#19152,#16022,#16023);
#12709=AXIS2_PLACEMENT_3D('',#19158,#16027,#16028);
#12710=AXIS2_PLACEMENT_3D('',#19164,#16032,#16033);
#12711=AXIS2_PLACEMENT_3D('',#19170,#16037,#16038);
#12712=AXIS2_PLACEMENT_3D('',#19173,#16041,#16042);
#12713=AXIS2_PLACEMENT_3D('',#19174,#16043,#16044);
#12714=AXIS2_PLACEMENT_3D('',#19175,#16045,#16046);
#12715=AXIS2_PLACEMENT_3D('',#19176,#16047,#16048);
#12716=AXIS2_PLACEMENT_3D('',#19177,#16049,#16050);
#12717=AXIS2_PLACEMENT_3D('',#19178,#16051,#16052);
#12718=AXIS2_PLACEMENT_3D('',#19179,#16053,#16054);
#12719=AXIS2_PLACEMENT_3D('',#19180,#16055,#16056);
#12720=AXIS2_PLACEMENT_3D('',#19181,#16057,#16058);
#12721=AXIS2_PLACEMENT_3D('',#19182,#16059,#16060);
#12722=AXIS2_PLACEMENT_3D('',#19183,#16061,#16062);
#12723=AXIS2_PLACEMENT_3D('',#19184,#16063,#16064);
#12724=AXIS2_PLACEMENT_3D('',#19185,#16065,#16066);
#12725=AXIS2_PLACEMENT_3D('',#19186,#16067,#16068);
#12726=AXIS2_PLACEMENT_3D('',#19187,#16069,#16070);
#12727=AXIS2_PLACEMENT_3D('',#19188,#16071,#16072);
#12728=DIRECTION('axis',(0.,0.,1.));
#12729=DIRECTION('refdir',(1.,0.,0.));
#12730=DIRECTION('axis',(0.,0.,1.));
#12731=DIRECTION('refdir',(1.,0.,0.));
#12732=DIRECTION('center_axis',(0.,-1.,0.));
#12733=DIRECTION('ref_axis',(0.,0.,-1.));
#12734=DIRECTION('center_axis',(0.,1.,0.));
#12735=DIRECTION('ref_axis',(1.,0.,0.));
#12736=DIRECTION('center_axis',(-1.,0.,-2.09002244843475E-16));
#12737=DIRECTION('ref_axis',(-2.09002244843475E-16,0.,1.));
#12738=DIRECTION('center_axis',(0.,-1.,0.));
#12739=DIRECTION('ref_axis',(1.,0.,0.));
#12740=DIRECTION('center_axis',(0.,-1.,0.));
#12741=DIRECTION('ref_axis',(1.,0.,0.));
#12742=DIRECTION('center_axis',(0.,-1.,0.));
#12743=DIRECTION('ref_axis',(1.,0.,0.));
#12744=DIRECTION('',(0.,1.,0.));
#12745=DIRECTION('center_axis',(0.,1.,0.));
#12746=DIRECTION('ref_axis',(1.,0.,0.));
#12747=DIRECTION('center_axis',(0.,1.,0.));
#12748=DIRECTION('ref_axis',(1.,0.,0.));
#12749=DIRECTION('center_axis',(0.,-1.,0.));
#12750=DIRECTION('ref_axis',(1.,0.,0.));
#12751=DIRECTION('center_axis',(0.,-1.,0.));
#12752=DIRECTION('ref_axis',(0.,0.,-1.));
#12753=DIRECTION('center_axis',(-1.,0.,-2.09002244843475E-16));
#12754=DIRECTION('ref_axis',(-2.09002244843475E-16,0.,1.));
#12755=DIRECTION('center_axis',(0.,1.,0.));
#12756=DIRECTION('ref_axis',(1.,0.,0.));
#12757=DIRECTION('center_axis',(0.,-1.,0.));
#12758=DIRECTION('ref_axis',(0.,0.,-1.));
#12759=DIRECTION('center_axis',(0.,1.,0.));
#12760=DIRECTION('ref_axis',(1.,0.,0.));
#12761=DIRECTION('center_axis',(-1.,0.,-2.09002244843475E-16));
#12762=DIRECTION('ref_axis',(-2.09002244843475E-16,0.,1.));
#12763=DIRECTION('center_axis',(0.,1.,0.));
#12764=DIRECTION('ref_axis',(1.,0.,0.));
#12765=DIRECTION('center_axis',(0.,1.,0.));
#12766=DIRECTION('ref_axis',(1.,0.,0.));
#12767=DIRECTION('center_axis',(0.,-1.,0.));
#12768=DIRECTION('ref_axis',(1.,0.,0.));
#12769=DIRECTION('center_axis',(0.,-1.,0.));
#12770=DIRECTION('ref_axis',(1.,0.,0.));
#12771=DIRECTION('',(0.,1.,0.));
#12772=DIRECTION('center_axis',(0.,-1.,0.));
#12773=DIRECTION('ref_axis',(1.,0.,0.));
#12774=DIRECTION('center_axis',(0.,-1.,0.));
#12775=DIRECTION('ref_axis',(0.,0.,-1.));
#12776=DIRECTION('center_axis',(-1.,0.,-2.09002244843475E-16));
#12777=DIRECTION('ref_axis',(-2.09002244843475E-16,0.,1.));
#12778=DIRECTION('center_axis',(0.,1.,0.));
#12779=DIRECTION('ref_axis',(-1.,0.,0.));
#12780=DIRECTION('center_axis',(0.,-1.,0.));
#12781=DIRECTION('ref_axis',(-1.,0.,0.));
#12782=DIRECTION('center_axis',(0.,1.,0.));
#12783=DIRECTION('ref_axis',(-1.,0.,0.));
#12784=DIRECTION('',(0.,-1.,0.));
#12785=DIRECTION('center_axis',(0.,-1.,0.));
#12786=DIRECTION('ref_axis',(-1.,0.,0.));
#12787=DIRECTION('center_axis',(0.,1.,0.));
#12788=DIRECTION('ref_axis',(0.,0.,1.));
#12789=DIRECTION('center_axis',(0.,-1.,0.));
#12790=DIRECTION('ref_axis',(1.,0.,0.));
#12791=DIRECTION('center_axis',(-1.,0.,2.09002244843475E-16));
#12792=DIRECTION('ref_axis',(-2.09002244843475E-16,0.,-1.));
#12793=DIRECTION('center_axis',(0.,1.,0.));
#12794=DIRECTION('ref_axis',(1.,0.,0.));
#12795=DIRECTION('center_axis',(0.,1.,0.));
#12796=DIRECTION('ref_axis',(1.,0.,0.));
#12797=DIRECTION('center_axis',(0.,1.,0.));
#12798=DIRECTION('ref_axis',(1.,0.,0.));
#12799=DIRECTION('',(0.,-1.,0.));
#12800=DIRECTION('center_axis',(0.,-1.,0.));
#12801=DIRECTION('ref_axis',(1.,0.,0.));
#12802=DIRECTION('center_axis',(0.,-1.,0.));
#12803=DIRECTION('ref_axis',(1.,0.,0.));
#12804=DIRECTION('center_axis',(0.,1.,0.));
#12805=DIRECTION('ref_axis',(1.,0.,0.));
#12806=DIRECTION('center_axis',(0.,-1.,0.));
#12807=DIRECTION('ref_axis',(0.,0.,-1.));
#12808=DIRECTION('center_axis',(-1.,0.,-2.09002244843475E-16));
#12809=DIRECTION('ref_axis',(-2.09002244843475E-16,0.,1.));
#12810=DIRECTION('axis',(0.,0.,1.));
#12811=DIRECTION('refdir',(1.,0.,0.));
#12812=DIRECTION('center_axis',(0.,1.,0.));
#12813=DIRECTION('ref_axis',(-1.,0.,0.));
#12814=DIRECTION('center_axis',(0.,1.,0.));
#12815=DIRECTION('ref_axis',(-1.,0.,0.));
#12816=DIRECTION('center_axis',(0.,1.,0.));
#12817=DIRECTION('ref_axis',(-1.,0.,0.));
#12818=DIRECTION('center_axis',(0.,1.,0.));
#12819=DIRECTION('ref_axis',(-1.,0.,0.));
#12820=DIRECTION('',(0.,-1.,0.));
#12821=DIRECTION('center_axis',(0.,1.,0.));
#12822=DIRECTION('ref_axis',(-1.,0.,0.));
#12823=DIRECTION('center_axis',(0.,1.,0.));
#12824=DIRECTION('ref_axis',(-1.,0.,0.));
#12825=DIRECTION('center_axis',(0.,1.,0.));
#12826=DIRECTION('ref_axis',(-1.,0.,0.));
#12827=DIRECTION('center_axis',(0.,1.,0.));
#12828=DIRECTION('ref_axis',(-1.,0.,0.));
#12829=DIRECTION('center_axis',(0.,1.,0.));
#12830=DIRECTION('ref_axis',(-1.,0.,0.));
#12831=DIRECTION('center_axis',(0.,1.,0.));
#12832=DIRECTION('ref_axis',(-1.,0.,0.));
#12833=DIRECTION('center_axis',(0.,1.,0.));
#12834=DIRECTION('ref_axis',(-1.,0.,0.));
#12835=DIRECTION('center_axis',(0.,1.,0.));
#12836=DIRECTION('ref_axis',(-1.,0.,0.));
#12837=DIRECTION('center_axis',(0.,-1.,0.));
#12838=DIRECTION('ref_axis',(-1.,0.,0.));
#12839=DIRECTION('center_axis',(0.,1.,0.));
#12840=DIRECTION('ref_axis',(-1.,0.,0.));
#12841=DIRECTION('',(0.,-1.,0.));
#12842=DIRECTION('center_axis',(0.,-1.,0.));
#12843=DIRECTION('ref_axis',(-1.,0.,0.));
#12844=DIRECTION('',(0.,1.,0.));
#12845=DIRECTION('center_axis',(0.,1.,0.));
#12846=DIRECTION('ref_axis',(-1.,0.,0.));
#12847=DIRECTION('center_axis',(0.,1.,0.));
#12848=DIRECTION('ref_axis',(-1.,0.,0.));
#12849=DIRECTION('center_axis',(0.,1.,0.));
#12850=DIRECTION('ref_axis',(-1.,0.,0.));
#12851=DIRECTION('center_axis',(0.,1.,0.));
#12852=DIRECTION('ref_axis',(-1.,0.,0.));
#12853=DIRECTION('center_axis',(0.,1.,0.));
#12854=DIRECTION('ref_axis',(-1.,0.,0.));
#12855=DIRECTION('',(0.,-1.,0.));
#12856=DIRECTION('center_axis',(0.,1.,0.));
#12857=DIRECTION('ref_axis',(-1.,0.,0.));
#12858=DIRECTION('center_axis',(0.,-1.,0.));
#12859=DIRECTION('ref_axis',(-1.,0.,0.));
#12860=DIRECTION('center_axis',(0.,-1.,0.));
#12861=DIRECTION('ref_axis',(-1.,0.,0.));
#12862=DIRECTION('',(0.,1.,0.));
#12863=DIRECTION('center_axis',(0.,-1.,0.));
#12864=DIRECTION('ref_axis',(-1.,0.,0.));
#12865=DIRECTION('center_axis',(0.,-1.,0.));
#12866=DIRECTION('ref_axis',(-1.,0.,0.));
#12867=DIRECTION('center_axis',(0.,-1.,0.));
#12868=DIRECTION('ref_axis',(-1.,0.,0.));
#12869=DIRECTION('',(0.,1.,0.));
#12870=DIRECTION('center_axis',(0.,-1.,0.));
#12871=DIRECTION('ref_axis',(-1.,0.,0.));
#12872=DIRECTION('',(0.,1.,0.));
#12873=DIRECTION('center_axis',(0.,1.,0.));
#12874=DIRECTION('ref_axis',(-1.,0.,0.));
#12875=DIRECTION('center_axis',(0.,1.,0.));
#12876=DIRECTION('ref_axis',(-1.,0.,0.));
#12877=DIRECTION('center_axis',(0.,-1.,0.));
#12878=DIRECTION('ref_axis',(-1.,0.,0.));
#12879=DIRECTION('center_axis',(0.,1.,0.));
#12880=DIRECTION('ref_axis',(-1.,0.,0.));
#12881=DIRECTION('',(0.,1.,0.));
#12882=DIRECTION('center_axis',(0.,1.,0.));
#12883=DIRECTION('ref_axis',(-1.,0.,0.));
#12884=DIRECTION('axis',(0.,0.,1.));
#12885=DIRECTION('refdir',(1.,0.,0.));
#12886=DIRECTION('center_axis',(0.,1.,0.));
#12887=DIRECTION('ref_axis',(-0.707106781186548,0.,-0.707106781186548));
#12888=DIRECTION('center_axis',(0.,-1.,0.));
#12889=DIRECTION('ref_axis',(-0.707106781186548,0.,-0.707106781186548));
#12890=DIRECTION('',(0.,-1.,0.));
#12891=DIRECTION('center_axis',(0.,1.,0.));
#12892=DIRECTION('ref_axis',(-0.707106781186548,0.,-0.707106781186548));
#12893=DIRECTION('',(0.,1.,0.));
#12894=DIRECTION('center_axis',(-1.,0.,0.));
#12895=DIRECTION('ref_axis',(0.,0.,1.));
#12896=DIRECTION('',(0.,0.,-1.));
#12897=DIRECTION('',(0.,-1.,0.));
#12898=DIRECTION('',(0.,0.,1.));
#12899=DIRECTION('center_axis',(1.,0.,0.));
#12900=DIRECTION('ref_axis',(2.22044604925031E-16,0.,1.));
#12901=DIRECTION('center_axis',(1.,0.,0.));
#12902=DIRECTION('ref_axis',(2.22044604925031E-16,0.,1.));
#12903=DIRECTION('center_axis',(1.,0.,0.));
#12904=DIRECTION('ref_axis',(2.22044604925031E-16,0.,1.));
#12905=DIRECTION('center_axis',(1.,0.,0.));
#12906=DIRECTION('ref_axis',(2.22044604925031E-16,0.,1.));
#12907=DIRECTION('center_axis',(1.,0.,0.));
#12908=DIRECTION('ref_axis',(2.22044604925031E-16,0.,1.));
#12909=DIRECTION('center_axis',(1.,0.,0.));
#12910=DIRECTION('ref_axis',(2.22044604925031E-16,0.,1.));
#12911=DIRECTION('center_axis',(1.,0.,0.));
#12912=DIRECTION('ref_axis',(2.22044604925031E-16,0.,1.));
#12913=DIRECTION('center_axis',(1.,0.,0.));
#12914=DIRECTION('ref_axis',(2.22044604925031E-16,0.,1.));
#12915=DIRECTION('center_axis',(1.,0.,0.));
#12916=DIRECTION('ref_axis',(2.22044604925031E-16,0.,1.));
#12917=DIRECTION('center_axis',(1.,0.,0.));
#12918=DIRECTION('ref_axis',(2.22044604925031E-16,0.,1.));
#12919=DIRECTION('center_axis',(1.,0.,0.));
#12920=DIRECTION('ref_axis',(2.22044604925031E-16,0.,1.));
#12921=DIRECTION('center_axis',(0.,1.,0.));
#12922=DIRECTION('ref_axis',(1.,0.,0.));
#12923=DIRECTION('',(1.,0.,0.));
#12924=DIRECTION('',(0.,0.,1.));
#12925=DIRECTION('',(1.,0.,4.89653224666665E-17));
#12926=DIRECTION('',(5.18929031489969E-17,0.,-1.));
#12927=DIRECTION('',(-1.,0.,0.));
#12928=DIRECTION('',(0.,0.,1.));
#12929=DIRECTION('',(-1.,0.,0.));
#12930=DIRECTION('center_axis',(0.,1.,0.));
#12931=DIRECTION('ref_axis',(-0.707106781186549,0.,0.707106781186546));
#12932=DIRECTION('center_axis',(0.,1.,0.));
#12933=DIRECTION('ref_axis',(-0.707106781186549,0.,0.707106781186546));
#12934=DIRECTION('center_axis',(0.,-1.,0.));
#12935=DIRECTION('ref_axis',(-0.707106781186549,0.,0.707106781186546));
#12936=DIRECTION('',(0.,1.,0.));
#12937=DIRECTION('center_axis',(0.,0.,-1.));
#12938=DIRECTION('ref_axis',(-1.,0.,0.));
#12939=DIRECTION('center_axis',(4.89653224666665E-17,0.,-1.));
#12940=DIRECTION('ref_axis',(-1.,0.,0.));
#12941=DIRECTION('',(0.,0.,-1.));
#12942=DIRECTION('center_axis',(0.,0.,1.));
#12943=DIRECTION('ref_axis',(-1.,0.,0.));
#12944=DIRECTION('center_axis',(0.,0.,-1.));
#12945=DIRECTION('ref_axis',(-1.,0.,0.));
#12946=DIRECTION('center_axis',(4.89653224666665E-17,0.,-1.));
#12947=DIRECTION('ref_axis',(-1.,0.,0.));
#12948=DIRECTION('',(0.,0.,-1.));
#12949=DIRECTION('center_axis',(0.,0.,1.));
#12950=DIRECTION('ref_axis',(-1.,0.,0.));
#12951=DIRECTION('center_axis',(0.,0.,-1.));
#12952=DIRECTION('ref_axis',(-1.,0.,0.));
#12953=DIRECTION('center_axis',(4.89653224666665E-17,0.,-1.));
#12954=DIRECTION('ref_axis',(-1.,0.,0.));
#12955=DIRECTION('',(0.,0.,-1.));
#12956=DIRECTION('center_axis',(0.,0.,1.));
#12957=DIRECTION('ref_axis',(-1.,0.,0.));
#12958=DIRECTION('center_axis',(0.,0.,-1.));
#12959=DIRECTION('ref_axis',(-1.,0.,0.));
#12960=DIRECTION('center_axis',(4.89653224666665E-17,0.,-1.));
#12961=DIRECTION('ref_axis',(-1.,0.,0.));
#12962=DIRECTION('',(0.,0.,-1.));
#12963=DIRECTION('center_axis',(0.,0.,1.));
#12964=DIRECTION('ref_axis',(-1.,0.,0.));
#12965=DIRECTION('center_axis',(0.,0.,-1.));
#12966=DIRECTION('ref_axis',(-1.,0.,0.));
#12967=DIRECTION('center_axis',(4.89653224666665E-17,0.,-1.));
#12968=DIRECTION('ref_axis',(-1.,0.,0.));
#12969=DIRECTION('',(0.,0.,-1.));
#12970=DIRECTION('center_axis',(0.,0.,1.));
#12971=DIRECTION('ref_axis',(-1.,0.,0.));
#12972=DIRECTION('center_axis',(0.,0.,-1.));
#12973=DIRECTION('ref_axis',(-1.,0.,0.));
#12974=DIRECTION('center_axis',(4.89653224666665E-17,0.,-1.));
#12975=DIRECTION('ref_axis',(-1.,0.,0.));
#12976=DIRECTION('',(0.,0.,-1.));
#12977=DIRECTION('center_axis',(0.,0.,1.));
#12978=DIRECTION('ref_axis',(-1.,0.,0.));
#12979=DIRECTION('center_axis',(0.,0.,-1.));
#12980=DIRECTION('ref_axis',(-1.,0.,0.));
#12981=DIRECTION('center_axis',(4.89653224666665E-17,0.,-1.));
#12982=DIRECTION('ref_axis',(-1.,0.,0.));
#12983=DIRECTION('',(0.,0.,-1.));
#12984=DIRECTION('center_axis',(0.,0.,1.));
#12985=DIRECTION('ref_axis',(-1.,0.,0.));
#12986=DIRECTION('center_axis',(0.,0.,-1.));
#12987=DIRECTION('ref_axis',(-1.,0.,0.));
#12988=DIRECTION('center_axis',(4.89653224666665E-17,0.,-1.));
#12989=DIRECTION('ref_axis',(-1.,0.,0.));
#12990=DIRECTION('',(0.,0.,-1.));
#12991=DIRECTION('center_axis',(0.,0.,1.));
#12992=DIRECTION('ref_axis',(-1.,0.,0.));
#12993=DIRECTION('center_axis',(0.,0.,-1.));
#12994=DIRECTION('ref_axis',(-1.,0.,0.));
#12995=DIRECTION('center_axis',(4.89653224666665E-17,0.,-1.));
#12996=DIRECTION('ref_axis',(-1.,0.,0.));
#12997=DIRECTION('',(0.,0.,-1.));
#12998=DIRECTION('center_axis',(0.,0.,1.));
#12999=DIRECTION('ref_axis',(-1.,0.,0.));
#13000=DIRECTION('center_axis',(0.,0.,-1.));
#13001=DIRECTION('ref_axis',(-1.,0.,0.));
#13002=DIRECTION('center_axis',(4.89653224666665E-17,0.,-1.));
#13003=DIRECTION('ref_axis',(-1.,0.,0.));
#13004=DIRECTION('',(0.,0.,-1.));
#13005=DIRECTION('center_axis',(0.,0.,1.));
#13006=DIRECTION('ref_axis',(-1.,0.,0.));
#13007=DIRECTION('center_axis',(0.,0.,-1.));
#13008=DIRECTION('ref_axis',(-1.,0.,0.));
#13009=DIRECTION('center_axis',(4.89653224666665E-17,0.,-1.));
#13010=DIRECTION('ref_axis',(-1.,0.,0.));
#13011=DIRECTION('',(0.,0.,-1.));
#13012=DIRECTION('center_axis',(0.,0.,1.));
#13013=DIRECTION('ref_axis',(-1.,0.,0.));
#13014=DIRECTION('center_axis',(-1.,0.,-2.22044604925031E-16));
#13015=DIRECTION('ref_axis',(2.22044604925031E-16,0.,1.));
#13016=DIRECTION('',(1.,0.,2.22044604925031E-16));
#13017=DIRECTION('center_axis',(-1.,0.,-5.18929031489969E-17));
#13018=DIRECTION('ref_axis',(2.22044604925031E-16,0.,1.));
#13019=DIRECTION('center_axis',(-1.,0.,-2.22044604925031E-16));
#13020=DIRECTION('ref_axis',(2.22044604925031E-16,0.,1.));
#13021=DIRECTION('',(1.,0.,2.22044604925031E-16));
#13022=DIRECTION('center_axis',(-1.,0.,-5.18929031489969E-17));
#13023=DIRECTION('ref_axis',(2.22044604925031E-16,0.,1.));
#13024=DIRECTION('center_axis',(-1.,0.,-2.22044604925031E-16));
#13025=DIRECTION('ref_axis',(2.22044604925031E-16,0.,1.));
#13026=DIRECTION('',(1.,0.,2.22044604925031E-16));
#13027=DIRECTION('center_axis',(-1.,0.,-5.18929031489969E-17));
#13028=DIRECTION('ref_axis',(2.22044604925031E-16,0.,1.));
#13029=DIRECTION('center_axis',(-1.,0.,-2.22044604925031E-16));
#13030=DIRECTION('ref_axis',(2.22044604925031E-16,0.,1.));
#13031=DIRECTION('',(1.,0.,2.22044604925031E-16));
#13032=DIRECTION('center_axis',(-1.,0.,-5.18929031489969E-17));
#13033=DIRECTION('ref_axis',(2.22044604925031E-16,0.,1.));
#13034=DIRECTION('center_axis',(-1.,0.,-2.22044604925031E-16));
#13035=DIRECTION('ref_axis',(2.22044604925031E-16,0.,1.));
#13036=DIRECTION('',(1.,0.,2.22044604925031E-16));
#13037=DIRECTION('center_axis',(-1.,0.,-5.18929031489969E-17));
#13038=DIRECTION('ref_axis',(2.22044604925031E-16,0.,1.));
#13039=DIRECTION('center_axis',(-1.,0.,-2.22044604925031E-16));
#13040=DIRECTION('ref_axis',(2.22044604925031E-16,0.,1.));
#13041=DIRECTION('',(1.,0.,2.22044604925031E-16));
#13042=DIRECTION('center_axis',(-1.,0.,-5.18929031489969E-17));
#13043=DIRECTION('ref_axis',(2.22044604925031E-16,0.,1.));
#13044=DIRECTION('center_axis',(-1.,0.,-2.22044604925031E-16));
#13045=DIRECTION('ref_axis',(2.22044604925031E-16,0.,1.));
#13046=DIRECTION('',(1.,0.,2.22044604925031E-16));
#13047=DIRECTION('center_axis',(-1.,0.,-5.18929031489969E-17));
#13048=DIRECTION('ref_axis',(2.22044604925031E-16,0.,1.));
#13049=DIRECTION('center_axis',(-1.,0.,-2.22044604925031E-16));
#13050=DIRECTION('ref_axis',(2.22044604925031E-16,0.,1.));
#13051=DIRECTION('',(1.,0.,2.22044604925031E-16));
#13052=DIRECTION('center_axis',(-1.,0.,-5.18929031489969E-17));
#13053=DIRECTION('ref_axis',(2.22044604925031E-16,0.,1.));
#13054=DIRECTION('center_axis',(-1.,0.,-2.22044604925031E-16));
#13055=DIRECTION('ref_axis',(2.22044604925031E-16,0.,1.));
#13056=DIRECTION('',(1.,0.,2.22044604925031E-16));
#13057=DIRECTION('center_axis',(-1.,0.,-5.18929031489969E-17));
#13058=DIRECTION('ref_axis',(2.22044604925031E-16,0.,1.));
#13059=DIRECTION('center_axis',(-1.,0.,-2.22044604925031E-16));
#13060=DIRECTION('ref_axis',(2.22044604925031E-16,0.,1.));
#13061=DIRECTION('',(1.,0.,2.22044604925031E-16));
#13062=DIRECTION('center_axis',(-1.,0.,-5.18929031489969E-17));
#13063=DIRECTION('ref_axis',(2.22044604925031E-16,0.,1.));
#13064=DIRECTION('center_axis',(-1.,0.,-2.22044604925031E-16));
#13065=DIRECTION('ref_axis',(2.22044604925031E-16,0.,1.));
#13066=DIRECTION('',(1.,0.,2.22044604925031E-16));
#13067=DIRECTION('center_axis',(-1.,0.,-5.18929031489969E-17));
#13068=DIRECTION('ref_axis',(2.22044604925031E-16,0.,1.));
#13069=DIRECTION('center_axis',(0.,0.,-1.));
#13070=DIRECTION('ref_axis',(-1.,0.,0.));
#13071=DIRECTION('center_axis',(0.,0.,-1.));
#13072=DIRECTION('ref_axis',(-1.,0.,0.));
#13073=DIRECTION('',(0.,0.,-1.));
#13074=DIRECTION('center_axis',(0.,0.,1.));
#13075=DIRECTION('ref_axis',(-1.,0.,0.));
#13076=DIRECTION('center_axis',(0.,0.,-1.));
#13077=DIRECTION('ref_axis',(-1.,0.,0.));
#13078=DIRECTION('center_axis',(0.,0.,-1.));
#13079=DIRECTION('ref_axis',(-1.,0.,0.));
#13080=DIRECTION('',(0.,0.,-1.));
#13081=DIRECTION('center_axis',(0.,0.,1.));
#13082=DIRECTION('ref_axis',(-1.,0.,0.));
#13083=DIRECTION('center_axis',(0.,0.,-1.));
#13084=DIRECTION('ref_axis',(-1.,0.,0.));
#13085=DIRECTION('center_axis',(0.,0.,-1.));
#13086=DIRECTION('ref_axis',(-1.,0.,0.));
#13087=DIRECTION('',(0.,0.,-1.));
#13088=DIRECTION('center_axis',(0.,0.,1.));
#13089=DIRECTION('ref_axis',(-1.,0.,0.));
#13090=DIRECTION('center_axis',(0.,0.,-1.));
#13091=DIRECTION('ref_axis',(-1.,0.,0.));
#13092=DIRECTION('center_axis',(0.,0.,-1.));
#13093=DIRECTION('ref_axis',(-1.,0.,0.));
#13094=DIRECTION('',(0.,0.,-1.));
#13095=DIRECTION('center_axis',(0.,0.,1.));
#13096=DIRECTION('ref_axis',(-1.,0.,0.));
#13097=DIRECTION('center_axis',(0.,0.,-1.));
#13098=DIRECTION('ref_axis',(-1.,0.,0.));
#13099=DIRECTION('center_axis',(0.,0.,-1.));
#13100=DIRECTION('ref_axis',(-1.,0.,0.));
#13101=DIRECTION('',(0.,0.,-1.));
#13102=DIRECTION('center_axis',(0.,0.,1.));
#13103=DIRECTION('ref_axis',(-1.,0.,0.));
#13104=DIRECTION('center_axis',(0.,0.,-1.));
#13105=DIRECTION('ref_axis',(-1.,0.,0.));
#13106=DIRECTION('center_axis',(0.,0.,-1.));
#13107=DIRECTION('ref_axis',(-1.,0.,0.));
#13108=DIRECTION('',(0.,0.,-1.));
#13109=DIRECTION('center_axis',(0.,0.,1.));
#13110=DIRECTION('ref_axis',(-1.,0.,0.));
#13111=DIRECTION('center_axis',(0.,0.,-1.));
#13112=DIRECTION('ref_axis',(-1.,0.,0.));
#13113=DIRECTION('center_axis',(0.,0.,-1.));
#13114=DIRECTION('ref_axis',(-1.,0.,0.));
#13115=DIRECTION('',(0.,0.,-1.));
#13116=DIRECTION('center_axis',(0.,0.,1.));
#13117=DIRECTION('ref_axis',(-1.,0.,0.));
#13118=DIRECTION('center_axis',(0.,0.,-1.));
#13119=DIRECTION('ref_axis',(-1.,0.,0.));
#13120=DIRECTION('center_axis',(0.,0.,-1.));
#13121=DIRECTION('ref_axis',(-1.,0.,0.));
#13122=DIRECTION('',(0.,0.,-1.));
#13123=DIRECTION('center_axis',(0.,0.,1.));
#13124=DIRECTION('ref_axis',(-1.,0.,0.));
#13125=DIRECTION('center_axis',(0.,0.,-1.));
#13126=DIRECTION('ref_axis',(-1.,0.,0.));
#13127=DIRECTION('center_axis',(0.,0.,-1.));
#13128=DIRECTION('ref_axis',(-1.,0.,0.));
#13129=DIRECTION('',(0.,0.,-1.));
#13130=DIRECTION('center_axis',(0.,0.,1.));
#13131=DIRECTION('ref_axis',(-1.,0.,0.));
#13132=DIRECTION('center_axis',(0.,0.,-1.));
#13133=DIRECTION('ref_axis',(-1.,0.,0.));
#13134=DIRECTION('center_axis',(0.,0.,-1.));
#13135=DIRECTION('ref_axis',(-1.,0.,0.));
#13136=DIRECTION('',(0.,0.,-1.));
#13137=DIRECTION('center_axis',(0.,0.,1.));
#13138=DIRECTION('ref_axis',(-1.,0.,0.));
#13139=DIRECTION('center_axis',(0.,0.,-1.));
#13140=DIRECTION('ref_axis',(-1.,0.,0.));
#13141=DIRECTION('center_axis',(0.,0.,-1.));
#13142=DIRECTION('ref_axis',(-1.,0.,0.));
#13143=DIRECTION('',(0.,0.,-1.));
#13144=DIRECTION('center_axis',(0.,0.,1.));
#13145=DIRECTION('ref_axis',(-1.,0.,0.));
#13146=DIRECTION('center_axis',(1.,0.,0.));
#13147=DIRECTION('ref_axis',(0.,0.,-1.));
#13148=DIRECTION('',(0.,1.,0.));
#13149=DIRECTION('',(0.,0.,-1.));
#13150=DIRECTION('',(0.,1.,0.));
#13151=DIRECTION('center_axis',(0.,0.,1.));
#13152=DIRECTION('ref_axis',(1.,0.,0.));
#13153=DIRECTION('',(1.,0.,0.));
#13154=DIRECTION('center_axis',(0.,0.,-1.));
#13155=DIRECTION('ref_axis',(-1.,0.,0.));
#13156=DIRECTION('',(-1.,0.,0.));
#13157=DIRECTION('',(0.,1.,0.));
#13158=DIRECTION('center_axis',(1.,0.,0.));
#13159=DIRECTION('ref_axis',(0.,0.,-1.));
#13160=DIRECTION('',(0.,0.,-1.));
#13161=DIRECTION('',(0.,1.,0.));
#13162=DIRECTION('center_axis',(-4.89653224666665E-17,0.,1.));
#13163=DIRECTION('ref_axis',(1.,0.,4.89653224666665E-17));
#13164=DIRECTION('',(1.,0.,4.89653224666665E-17));
#13165=DIRECTION('',(0.,1.,0.));
#13166=DIRECTION('center_axis',(1.,0.,5.18929031489969E-17));
#13167=DIRECTION('ref_axis',(5.18929031489969E-17,0.,-1.));
#13168=DIRECTION('',(5.18929031489969E-17,0.,-1.));
#13169=DIRECTION('',(0.,1.,0.));
#13170=DIRECTION('center_axis',(0.,0.,-1.));
#13171=DIRECTION('ref_axis',(-1.,0.,0.));
#13172=DIRECTION('',(-1.,0.,0.));
#13173=DIRECTION('center_axis',(0.,1.,0.));
#13174=DIRECTION('ref_axis',(0.,0.,1.));
#13175=DIRECTION('axis',(0.,0.,1.));
#13176=DIRECTION('refdir',(1.,0.,0.));
#13177=DIRECTION('center_axis',(0.,-1.,0.));
#13178=DIRECTION('ref_axis',(1.,0.,0.));
#13179=DIRECTION('',(0.427641188232285,0.,0.903948568297599));
#13180=DIRECTION('',(0.996663017976436,0.,0.0816261514350802));
#13181=DIRECTION('',(0.569021829744153,0.,-0.82232241686252));
#13182=DIRECTION('',(-0.427641188232283,0.,-0.9039485682976));
#13183=DIRECTION('',(-0.996663017976436,0.,-0.0816261514350783));
#13184=DIRECTION('',(-0.569021829744152,0.,0.822322416862521));
#13185=DIRECTION('center_axis',(0.,1.,0.));
#13186=DIRECTION('ref_axis',(1.,0.,0.));
#13187=DIRECTION('center_axis',(0.0816261514350802,0.,-0.996663017976436));
#13188=DIRECTION('ref_axis',(0.996663017976436,0.,0.0816261514350802));
#13189=DIRECTION('',(0.,-1.,0.));
#13190=DIRECTION('',(0.996663017976436,0.,0.0816261514350802));
#13191=DIRECTION('',(0.,-1.,0.));
#13192=DIRECTION('center_axis',(-0.82232241686252,0.,-0.569021829744153));
#13193=DIRECTION('ref_axis',(0.569021829744153,0.,-0.82232241686252));
#13194=DIRECTION('',(0.569021829744153,0.,-0.82232241686252));
#13195=DIRECTION('',(0.,-1.,0.));
#13196=DIRECTION('center_axis',(-0.9039485682976,0.,0.427641188232283));
#13197=DIRECTION('ref_axis',(-0.427641188232283,0.,-0.9039485682976));
#13198=DIRECTION('',(-0.427641188232283,0.,-0.9039485682976));
#13199=DIRECTION('',(0.,-1.,0.));
#13200=DIRECTION('center_axis',(-0.0816261514350783,0.,0.996663017976436));
#13201=DIRECTION('ref_axis',(-0.996663017976436,0.,-0.0816261514350783));
#13202=DIRECTION('',(-0.996663017976436,0.,-0.0816261514350783));
#13203=DIRECTION('',(0.,-1.,0.));
#13204=DIRECTION('center_axis',(0.822322416862521,0.,0.569021829744152));
#13205=DIRECTION('ref_axis',(-0.569021829744152,0.,0.822322416862521));
#13206=DIRECTION('',(-0.569021829744152,0.,0.822322416862521));
#13207=DIRECTION('',(0.,-1.,0.));
#13208=DIRECTION('center_axis',(0.903948568297599,0.,-0.427641188232285));
#13209=DIRECTION('ref_axis',(0.427641188232285,0.,0.903948568297599));
#13210=DIRECTION('',(0.427641188232285,0.,0.903948568297599));
#13211=DIRECTION('center_axis',(0.,-1.,0.));
#13212=DIRECTION('ref_axis',(1.,0.,0.));
#13213=DIRECTION('center_axis',(0.,1.,0.));
#13214=DIRECTION('ref_axis',(1.,0.,0.));
#13215=DIRECTION('center_axis',(0.,1.,0.));
#13216=DIRECTION('ref_axis',(1.,0.,0.));
#13217=DIRECTION('',(0.,-1.,0.));
#13218=DIRECTION('center_axis',(0.,-1.,0.));
#13219=DIRECTION('ref_axis',(1.,0.,0.));
#13220=DIRECTION('axis',(0.,0.,1.));
#13221=DIRECTION('refdir',(1.,0.,0.));
#13222=DIRECTION('center_axis',(0.,-0.984725314960397,0.174115059877505));
#13223=DIRECTION('ref_axis',(0.,0.174115059877505,0.984725314960397));
#13224=DIRECTION('',(0.,-0.174115059877505,-0.984725314960397));
#13225=DIRECTION('',(-1.,0.,0.));
#13226=DIRECTION('',(0.,0.174115059877505,0.984725314960397));
#13227=DIRECTION('',(-1.,0.,0.));
#13228=DIRECTION('center_axis',(1.,0.,0.));
#13229=DIRECTION('ref_axis',(0.,-0.821913269381079,-0.569612655771715));
#13230=DIRECTION('center_axis',(-1.,0.,0.));
#13231=DIRECTION('ref_axis',(0.,-0.821913269381079,-0.569612655771715));
#13232=DIRECTION('',(-1.,0.,0.));
#13233=DIRECTION('center_axis',(-1.,0.,0.));
#13234=DIRECTION('ref_axis',(0.,-0.821913269381079,-0.569612655771715));
#13235=DIRECTION('center_axis',(0.,-0.821913269381085,-0.569612655771705));
#13236=DIRECTION('ref_axis',(0.,-0.569612655771705,0.821913269381085));
#13237=DIRECTION('',(0.,0.569612655771705,-0.821913269381085));
#13238=DIRECTION('',(1.,0.,0.));
#13239=DIRECTION('',(0.,-0.569612655771705,0.821913269381085));
#13240=DIRECTION('center_axis',(0.,0.821913269381085,0.569612655771706));
#13241=DIRECTION('ref_axis',(0.,0.569612655771706,-0.821913269381085));
#13242=DIRECTION('',(0.,0.569612655771706,-0.821913269381085));
#13243=DIRECTION('',(-1.,0.,0.));
#13244=DIRECTION('',(0.,0.569612655771706,-0.821913269381085));
#13245=DIRECTION('',(-1.,0.,0.));
#13246=DIRECTION('center_axis',(1.,0.,0.));
#13247=DIRECTION('ref_axis',(0.,-0.821913269381079,-0.569612655771714));
#13248=DIRECTION('center_axis',(-1.,0.,0.));
#13249=DIRECTION('ref_axis',(0.,-0.821913269381079,-0.569612655771714));
#13250=DIRECTION('',(-1.,0.,0.));
#13251=DIRECTION('center_axis',(1.,0.,0.));
#13252=DIRECTION('ref_axis',(0.,-0.821913269381079,-0.569612655771714));
#13253=DIRECTION('center_axis',(0.,0.984725314960397,-0.174115059877505));
#13254=DIRECTION('ref_axis',(0.,-0.174115059877505,-0.984725314960397));
#13255=DIRECTION('',(0.,-0.174115059877505,-0.984725314960397));
#13256=DIRECTION('',(-1.,0.,0.));
#13257=DIRECTION('',(0.,-0.174115059877505,-0.984725314960397));
#13258=DIRECTION('center_axis',(1.,0.,0.));
#13259=DIRECTION('ref_axis',(0.,8.88178419700113E-15,1.));
#13260=DIRECTION('center_axis',(-1.,0.,0.));
#13261=DIRECTION('ref_axis',(0.,8.88178419700113E-15,1.));
#13262=DIRECTION('',(-1.,0.,0.));
#13263=DIRECTION('center_axis',(-1.,0.,0.));
#13264=DIRECTION('ref_axis',(0.,8.88178419700113E-15,1.));
#13265=DIRECTION('center_axis',(1.,0.,0.));
#13266=DIRECTION('ref_axis',(0.,0.,1.));
#13267=DIRECTION('center_axis',(-1.,0.,0.));
#13268=DIRECTION('ref_axis',(0.,0.,1.));
#13269=DIRECTION('center_axis',(1.,0.,0.));
#13270=DIRECTION('ref_axis',(0.,0.,1.));
#13271=DIRECTION('',(-1.,0.,0.));
#13272=DIRECTION('center_axis',(0.,-6.91402766832813E-16,-1.));
#13273=DIRECTION('ref_axis',(0.,-1.,6.91402766832813E-16));
#13274=DIRECTION('',(0.,-1.,6.91402766832813E-16));
#13275=DIRECTION('',(-1.,0.,0.));
#13276=DIRECTION('',(0.,1.,6.91402766832813E-16));
#13277=DIRECTION('center_axis',(0.,-0.984725314960397,-0.174115059877505));
#13278=DIRECTION('ref_axis',(0.,-0.174115059877505,0.984725314960397));
#13279=DIRECTION('',(0.,0.174115059877505,-0.984725314960397));
#13280=DIRECTION('',(-1.,0.,0.));
#13281=DIRECTION('',(0.,-0.174115059877505,0.984725314960397));
#13282=DIRECTION('',(-1.,0.,0.));
#13283=DIRECTION('center_axis',(-1.,0.,0.));
#13284=DIRECTION('ref_axis',(0.,0.821913269381079,-0.569612655771715));
#13285=DIRECTION('center_axis',(1.,0.,0.));
#13286=DIRECTION('ref_axis',(0.,0.821913269381079,-0.569612655771715));
#13287=DIRECTION('center_axis',(1.,0.,0.));
#13288=DIRECTION('ref_axis',(0.,0.821913269381079,-0.569612655771715));
#13289=DIRECTION('',(-1.,0.,0.));
#13290=DIRECTION('center_axis',(0.,-0.821913269381085,0.569612655771705));
#13291=DIRECTION('ref_axis',(0.,0.569612655771705,0.821913269381085));
#13292=DIRECTION('',(0.,-0.569612655771705,-0.821913269381085));
#13293=DIRECTION('',(0.,0.569612655771705,0.821913269381085));
#13294=DIRECTION('',(-1.,0.,0.));
#13295=DIRECTION('center_axis',(0.,0.821913269381085,-0.569612655771706));
#13296=DIRECTION('ref_axis',(0.,-0.569612655771706,-0.821913269381085));
#13297=DIRECTION('',(0.,-0.569612655771706,-0.821913269381085));
#13298=DIRECTION('',(1.,0.,0.));
#13299=DIRECTION('',(0.,-0.569612655771706,-0.821913269381085));
#13300=DIRECTION('',(-1.,0.,0.));
#13301=DIRECTION('center_axis',(-1.,0.,0.));
#13302=DIRECTION('ref_axis',(0.,0.821913269381079,-0.569612655771714));
#13303=DIRECTION('center_axis',(1.,0.,0.));
#13304=DIRECTION('ref_axis',(0.,0.821913269381079,-0.569612655771714));
#13305=DIRECTION('center_axis',(-1.,0.,0.));
#13306=DIRECTION('ref_axis',(0.,0.821913269381079,-0.569612655771714));
#13307=DIRECTION('',(-1.,0.,0.));
#13308=DIRECTION('center_axis',(0.,0.984725314960397,0.174115059877505));
#13309=DIRECTION('ref_axis',(0.,0.174115059877505,-0.984725314960397));
#13310=DIRECTION('',(0.,0.174115059877505,-0.984725314960397));
#13311=DIRECTION('',(0.,0.174115059877505,-0.984725314960397));
#13312=DIRECTION('',(-1.,0.,0.));
#13313=DIRECTION('center_axis',(-1.,0.,0.));
#13314=DIRECTION('ref_axis',(0.,-8.88178419700113E-15,1.));
#13315=DIRECTION('center_axis',(1.,0.,0.));
#13316=DIRECTION('ref_axis',(0.,-8.88178419700113E-15,1.));
#13317=DIRECTION('center_axis',(1.,0.,0.));
#13318=DIRECTION('ref_axis',(0.,-8.88178419700113E-15,1.));
#13319=DIRECTION('center_axis',(0.,0.,1.));
#13320=DIRECTION('ref_axis',(0.,1.,0.));
#13321=DIRECTION('',(0.,1.,0.));
#13322=DIRECTION('',(-1.,0.,0.));
#13323=DIRECTION('',(0.,-1.,0.));
#13324=DIRECTION('center_axis',(-1.,0.,0.));
#13325=DIRECTION('ref_axis',(0.,0.,1.));
#13326=DIRECTION('center_axis',(1.,0.,0.));
#13327=DIRECTION('ref_axis',(0.,0.,1.));
#13328=DIRECTION('center_axis',(-1.,0.,0.));
#13329=DIRECTION('ref_axis',(0.,0.,1.));
#13330=DIRECTION('center_axis',(0.,0.,1.));
#13331=DIRECTION('ref_axis',(0.,1.,0.));
#13332=DIRECTION('',(0.,1.,0.));
#13333=DIRECTION('',(-1.,0.,0.));
#13334=DIRECTION('',(0.,1.,0.));
#13335=DIRECTION('center_axis',(0.,0.,1.));
#13336=DIRECTION('ref_axis',(0.,1.,0.));
#13337=DIRECTION('',(0.,1.,0.));
#13338=DIRECTION('',(-1.,0.,0.));
#13339=DIRECTION('',(0.,1.,0.));
#13340=DIRECTION('center_axis',(0.,0.,1.));
#13341=DIRECTION('ref_axis',(0.,1.,0.));
#13342=DIRECTION('',(0.,1.,0.));
#13343=DIRECTION('',(0.,1.,0.));
#13344=DIRECTION('center_axis',(1.,0.,0.));
#13345=DIRECTION('ref_axis',(0.,0.707106781186555,-0.70710678118654));
#13346=DIRECTION('center_axis',(-1.,0.,0.));
#13347=DIRECTION('ref_axis',(0.,0.707106781186555,-0.70710678118654));
#13348=DIRECTION('',(-1.,0.,0.));
#13349=DIRECTION('center_axis',(-1.,0.,0.));
#13350=DIRECTION('ref_axis',(0.,0.707106781186555,-0.70710678118654));
#13351=DIRECTION('center_axis',(0.,0.707106781186548,-0.707106781186548));
#13352=DIRECTION('ref_axis',(0.,-0.707106781186548,-0.707106781186548));
#13353=DIRECTION('',(0.,0.707106781186547,0.707106781186547));
#13354=DIRECTION('',(-1.,0.,0.));
#13355=DIRECTION('',(0.,-0.707106781186547,-0.707106781186547));
#13356=DIRECTION('center_axis',(1.,0.,0.));
#13357=DIRECTION('ref_axis',(0.,0.98480775301221,-0.17364817766692));
#13358=DIRECTION('center_axis',(-1.,0.,0.));
#13359=DIRECTION('ref_axis',(0.,0.98480775301221,-0.17364817766692));
#13360=DIRECTION('',(-1.,0.,0.));
#13361=DIRECTION('center_axis',(-1.,0.,0.));
#13362=DIRECTION('ref_axis',(0.,0.98480775301221,-0.17364817766692));
#13363=DIRECTION('center_axis',(0.,0.984807753012208,-0.173648177666932));
#13364=DIRECTION('ref_axis',(0.,-0.173648177666932,-0.984807753012208));
#13365=DIRECTION('',(0.,0.173648177666932,0.984807753012208));
#13366=DIRECTION('',(-1.,0.,0.));
#13367=DIRECTION('',(0.,-0.173648177666932,-0.984807753012208));
#13368=DIRECTION('center_axis',(0.,0.,-1.));
#13369=DIRECTION('ref_axis',(0.,-1.,0.));
#13370=DIRECTION('',(0.,-1.,0.));
#13371=DIRECTION('',(-1.,0.,0.));
#13372=DIRECTION('',(0.,-1.,0.));
#13373=DIRECTION('center_axis',(0.,-0.984807753012208,0.173648177666932));
#13374=DIRECTION('ref_axis',(0.,0.173648177666932,0.984807753012208));
#13375=DIRECTION('',(0.,0.173648177666932,0.984807753012208));
#13376=DIRECTION('',(-1.,0.,0.));
#13377=DIRECTION('',(0.,0.173648177666932,0.984807753012208));
#13378=DIRECTION('center_axis',(1.,0.,0.));
#13379=DIRECTION('ref_axis',(0.,0.984807753012209,-0.173648177666926));
#13380=DIRECTION('center_axis',(-1.,0.,0.));
#13381=DIRECTION('ref_axis',(0.,0.984807753012209,-0.173648177666926));
#13382=DIRECTION('',(-1.,0.,0.));
#13383=DIRECTION('center_axis',(1.,0.,0.));
#13384=DIRECTION('ref_axis',(0.,0.984807753012209,-0.173648177666926));
#13385=DIRECTION('center_axis',(0.,-0.707106781186547,0.707106781186548));
#13386=DIRECTION('ref_axis',(0.,0.707106781186548,0.707106781186547));
#13387=DIRECTION('',(0.,0.707106781186548,0.707106781186547));
#13388=DIRECTION('',(-1.,0.,0.));
#13389=DIRECTION('',(0.,0.707106781186548,0.707106781186547));
#13390=DIRECTION('center_axis',(1.,0.,0.));
#13391=DIRECTION('ref_axis',(0.,0.707106781186551,-0.707106781186544));
#13392=DIRECTION('center_axis',(-1.,0.,0.));
#13393=DIRECTION('ref_axis',(0.,0.707106781186551,-0.707106781186544));
#13394=DIRECTION('',(-1.,0.,0.));
#13395=DIRECTION('center_axis',(1.,0.,0.));
#13396=DIRECTION('ref_axis',(0.,0.707106781186551,-0.707106781186544));
#13397=DIRECTION('center_axis',(0.,0.,-1.));
#13398=DIRECTION('ref_axis',(0.,-1.,0.));
#13399=DIRECTION('',(0.,-1.,0.));
#13400=DIRECTION('',(-1.,0.,0.));
#13401=DIRECTION('',(0.,1.,0.));
#13402=DIRECTION('center_axis',(-1.,0.,0.));
#13403=DIRECTION('ref_axis',(0.,-0.707106781186555,-0.70710678118654));
#13404=DIRECTION('center_axis',(1.,0.,0.));
#13405=DIRECTION('ref_axis',(0.,-0.707106781186555,-0.70710678118654));
#13406=DIRECTION('center_axis',(1.,0.,0.));
#13407=DIRECTION('ref_axis',(0.,-0.707106781186555,-0.70710678118654));
#13408=DIRECTION('',(-1.,0.,0.));
#13409=DIRECTION('center_axis',(0.,0.707106781186548,0.707106781186548));
#13410=DIRECTION('ref_axis',(0.,0.707106781186548,-0.707106781186548));
#13411=DIRECTION('',(0.,-0.707106781186547,0.707106781186547));
#13412=DIRECTION('',(0.,0.707106781186547,-0.707106781186547));
#13413=DIRECTION('',(-1.,0.,0.));
#13414=DIRECTION('center_axis',(-1.,0.,0.));
#13415=DIRECTION('ref_axis',(0.,-0.98480775301221,-0.17364817766692));
#13416=DIRECTION('center_axis',(1.,0.,0.));
#13417=DIRECTION('ref_axis',(0.,-0.98480775301221,-0.17364817766692));
#13418=DIRECTION('center_axis',(1.,0.,0.));
#13419=DIRECTION('ref_axis',(0.,-0.98480775301221,-0.17364817766692));
#13420=DIRECTION('',(-1.,0.,0.));
#13421=DIRECTION('center_axis',(0.,0.984807753012208,0.173648177666932));
#13422=DIRECTION('ref_axis',(0.,0.173648177666932,-0.984807753012208));
#13423=DIRECTION('',(0.,-0.173648177666932,0.984807753012208));
#13424=DIRECTION('',(0.,0.173648177666932,-0.984807753012208));
#13425=DIRECTION('',(-1.,0.,0.));
#13426=DIRECTION('center_axis',(0.,0.,1.));
#13427=DIRECTION('ref_axis',(0.,1.,0.));
#13428=DIRECTION('',(0.,1.,0.));
#13429=DIRECTION('',(0.,1.,0.));
#13430=DIRECTION('',(-1.,0.,0.));
#13431=DIRECTION('center_axis',(0.,-0.984807753012208,-0.173648177666932));
#13432=DIRECTION('ref_axis',(0.,-0.173648177666932,0.984807753012208));
#13433=DIRECTION('',(0.,-0.173648177666932,0.984807753012208));
#13434=DIRECTION('',(0.,-0.173648177666932,0.984807753012208));
#13435=DIRECTION('',(-1.,0.,0.));
#13436=DIRECTION('center_axis',(-1.,0.,0.));
#13437=DIRECTION('ref_axis',(0.,-0.984807753012209,-0.173648177666926));
#13438=DIRECTION('center_axis',(1.,0.,0.));
#13439=DIRECTION('ref_axis',(0.,-0.984807753012209,-0.173648177666926));
#13440=DIRECTION('center_axis',(-1.,0.,0.));
#13441=DIRECTION('ref_axis',(0.,-0.984807753012209,-0.173648177666926));
#13442=DIRECTION('',(-1.,0.,0.));
#13443=DIRECTION('center_axis',(0.,-0.707106781186547,-0.707106781186548));
#13444=DIRECTION('ref_axis',(0.,-0.707106781186548,0.707106781186547));
#13445=DIRECTION('',(0.,-0.707106781186548,0.707106781186547));
#13446=DIRECTION('',(0.,-0.707106781186548,0.707106781186547));
#13447=DIRECTION('',(-1.,0.,0.));
#13448=DIRECTION('center_axis',(-1.,0.,0.));
#13449=DIRECTION('ref_axis',(0.,-0.707106781186551,-0.707106781186544));
#13450=DIRECTION('center_axis',(1.,0.,0.));
#13451=DIRECTION('ref_axis',(0.,-0.707106781186551,-0.707106781186544));
#13452=DIRECTION('center_axis',(-1.,0.,0.));
#13453=DIRECTION('ref_axis',(0.,-0.707106781186551,-0.707106781186544));
#13454=DIRECTION('center_axis',(1.,0.,0.));
#13455=DIRECTION('ref_axis',(0.,1.,0.));
#13456=DIRECTION('center_axis',(1.,0.,0.));
#13457=DIRECTION('ref_axis',(0.,1.,0.));
#13458=DIRECTION('axis',(0.,0.,1.));
#13459=DIRECTION('refdir',(1.,0.,0.));
#13460=DIRECTION('center_axis',(0.,0.,-1.));
#13461=DIRECTION('ref_axis',(-1.,0.,0.));
#13462=DIRECTION('center_axis',(0.,0.,-1.));
#13463=DIRECTION('ref_axis',(-1.,0.,0.));
#13464=DIRECTION('',(0.,0.,-1.));
#13465=DIRECTION('center_axis',(0.,0.,1.));
#13466=DIRECTION('ref_axis',(-1.,0.,0.));
#13467=DIRECTION('center_axis',(0.,0.,-1.));
#13468=DIRECTION('ref_axis',(-1.,0.,0.));
#13469=DIRECTION('center_axis',(0.,0.,-1.));
#13470=DIRECTION('ref_axis',(-1.,0.,0.));
#13471=DIRECTION('',(0.,0.,-1.));
#13472=DIRECTION('center_axis',(0.,0.,1.));
#13473=DIRECTION('ref_axis',(-1.,0.,0.));
#13474=DIRECTION('center_axis',(0.,0.,-1.));
#13475=DIRECTION('ref_axis',(-1.,0.,0.));
#13476=DIRECTION('center_axis',(0.,0.,-1.));
#13477=DIRECTION('ref_axis',(-1.,0.,0.));
#13478=DIRECTION('',(0.,0.,-1.));
#13479=DIRECTION('center_axis',(0.,0.,1.));
#13480=DIRECTION('ref_axis',(-1.,0.,0.));
#13481=DIRECTION('center_axis',(0.,0.,-1.));
#13482=DIRECTION('ref_axis',(-1.,0.,0.));
#13483=DIRECTION('center_axis',(0.,0.,-1.));
#13484=DIRECTION('ref_axis',(-1.,0.,0.));
#13485=DIRECTION('',(0.,0.,-1.));
#13486=DIRECTION('center_axis',(0.,0.,1.));
#13487=DIRECTION('ref_axis',(-1.,0.,0.));
#13488=DIRECTION('center_axis',(0.,0.,-1.));
#13489=DIRECTION('ref_axis',(-1.,0.,0.));
#13490=DIRECTION('center_axis',(0.,0.,-1.));
#13491=DIRECTION('ref_axis',(-1.,0.,0.));
#13492=DIRECTION('',(0.,0.,-1.));
#13493=DIRECTION('center_axis',(0.,0.,1.));
#13494=DIRECTION('ref_axis',(-1.,0.,0.));
#13495=DIRECTION('center_axis',(-1.,0.,0.));
#13496=DIRECTION('ref_axis',(0.,1.,0.));
#13497=DIRECTION('',(0.,-1.,0.));
#13498=DIRECTION('',(0.,0.,-1.));
#13499=DIRECTION('',(0.,1.,0.));
#13500=DIRECTION('',(0.,0.,-1.));
#13501=DIRECTION('center_axis',(0.,0.,-1.));
#13502=DIRECTION('ref_axis',(-1.,0.,0.));
#13503=DIRECTION('center_axis',(0.,0.,1.));
#13504=DIRECTION('ref_axis',(-1.,0.,0.));
#13505=DIRECTION('center_axis',(0.,0.,-1.));
#13506=DIRECTION('ref_axis',(-1.,0.,0.));
#13507=DIRECTION('',(0.,0.,-1.));
#13508=DIRECTION('center_axis',(1.,0.,0.));
#13509=DIRECTION('ref_axis',(0.,-1.,0.));
#13510=DIRECTION('',(0.,1.,0.));
#13511=DIRECTION('',(0.,-1.,0.));
#13512=DIRECTION('',(0.,0.,-1.));
#13513=DIRECTION('center_axis',(0.,0.,-1.));
#13514=DIRECTION('ref_axis',(1.,0.,0.));
#13515=DIRECTION('center_axis',(0.,0.,1.));
#13516=DIRECTION('ref_axis',(1.,0.,0.));
#13517=DIRECTION('center_axis',(0.,0.,-1.));
#13518=DIRECTION('ref_axis',(1.,0.,0.));
#13519=DIRECTION('center_axis',(-1.,0.,0.));
#13520=DIRECTION('ref_axis',(0.,1.,0.));
#13521=DIRECTION('',(0.,-1.,0.));
#13522=DIRECTION('',(0.,0.,-1.));
#13523=DIRECTION('',(0.,1.,0.));
#13524=DIRECTION('',(0.,0.,-1.));
#13525=DIRECTION('center_axis',(0.,0.,-1.));
#13526=DIRECTION('ref_axis',(-1.,0.,0.));
#13527=DIRECTION('center_axis',(0.,0.,1.));
#13528=DIRECTION('ref_axis',(-1.,0.,0.));
#13529=DIRECTION('center_axis',(0.,0.,-1.));
#13530=DIRECTION('ref_axis',(-1.,0.,0.));
#13531=DIRECTION('',(0.,0.,-1.));
#13532=DIRECTION('center_axis',(1.,0.,0.));
#13533=DIRECTION('ref_axis',(0.,-1.,0.));
#13534=DIRECTION('',(0.,1.,0.));
#13535=DIRECTION('',(0.,-1.,0.));
#13536=DIRECTION('',(0.,0.,-1.));
#13537=DIRECTION('center_axis',(0.,0.,-1.));
#13538=DIRECTION('ref_axis',(1.,0.,0.));
#13539=DIRECTION('center_axis',(0.,0.,1.));
#13540=DIRECTION('ref_axis',(1.,0.,0.));
#13541=DIRECTION('center_axis',(0.,0.,-1.));
#13542=DIRECTION('ref_axis',(1.,0.,0.));
#13543=DIRECTION('center_axis',(0.,0.,-1.));
#13544=DIRECTION('ref_axis',(-1.,0.,0.));
#13545=DIRECTION('center_axis',(0.,0.,-1.));
#13546=DIRECTION('ref_axis',(-1.,0.,0.));
#13547=DIRECTION('',(0.,0.,-1.));
#13548=DIRECTION('center_axis',(0.,0.,1.));
#13549=DIRECTION('ref_axis',(-1.,0.,0.));
#13550=DIRECTION('center_axis',(0.,0.,-1.));
#13551=DIRECTION('ref_axis',(-1.,0.,0.));
#13552=DIRECTION('center_axis',(0.,0.,-1.));
#13553=DIRECTION('ref_axis',(-1.,0.,0.));
#13554=DIRECTION('',(0.,0.,-1.));
#13555=DIRECTION('center_axis',(0.,0.,1.));
#13556=DIRECTION('ref_axis',(-1.,0.,0.));
#13557=DIRECTION('center_axis',(0.,0.,-1.));
#13558=DIRECTION('ref_axis',(-1.,0.,0.));
#13559=DIRECTION('center_axis',(0.,0.,-1.));
#13560=DIRECTION('ref_axis',(-1.,0.,0.));
#13561=DIRECTION('',(0.,0.,-1.));
#13562=DIRECTION('center_axis',(0.,0.,1.));
#13563=DIRECTION('ref_axis',(-1.,0.,0.));
#13564=DIRECTION('center_axis',(0.,0.,-1.));
#13565=DIRECTION('ref_axis',(-1.,0.,0.));
#13566=DIRECTION('center_axis',(0.,0.,-1.));
#13567=DIRECTION('ref_axis',(-1.,0.,0.));
#13568=DIRECTION('',(0.,0.,-1.));
#13569=DIRECTION('center_axis',(0.,0.,1.));
#13570=DIRECTION('ref_axis',(-1.,0.,0.));
#13571=DIRECTION('center_axis',(0.,0.,-1.));
#13572=DIRECTION('ref_axis',(-1.,0.,0.));
#13573=DIRECTION('center_axis',(0.,0.,-1.));
#13574=DIRECTION('ref_axis',(-1.,0.,0.));
#13575=DIRECTION('',(0.,0.,-1.));
#13576=DIRECTION('center_axis',(0.,0.,1.));
#13577=DIRECTION('ref_axis',(-1.,0.,0.));
#13578=DIRECTION('center_axis',(-1.,0.,0.));
#13579=DIRECTION('ref_axis',(0.,1.,0.));
#13580=DIRECTION('',(0.,-1.,0.));
#13581=DIRECTION('',(0.,0.,-1.));
#13582=DIRECTION('',(0.,1.,0.));
#13583=DIRECTION('',(0.,0.,-1.));
#13584=DIRECTION('center_axis',(0.,0.,-1.));
#13585=DIRECTION('ref_axis',(-1.,0.,0.));
#13586=DIRECTION('center_axis',(0.,0.,1.));
#13587=DIRECTION('ref_axis',(-1.,0.,0.));
#13588=DIRECTION('center_axis',(0.,0.,-1.));
#13589=DIRECTION('ref_axis',(-1.,0.,0.));
#13590=DIRECTION('',(0.,0.,-1.));
#13591=DIRECTION('center_axis',(1.,0.,0.));
#13592=DIRECTION('ref_axis',(0.,-1.,0.));
#13593=DIRECTION('',(0.,1.,0.));
#13594=DIRECTION('',(0.,-1.,0.));
#13595=DIRECTION('',(0.,0.,-1.));
#13596=DIRECTION('center_axis',(0.,0.,-1.));
#13597=DIRECTION('ref_axis',(1.,0.,0.));
#13598=DIRECTION('center_axis',(0.,0.,1.));
#13599=DIRECTION('ref_axis',(1.,0.,0.));
#13600=DIRECTION('center_axis',(0.,0.,-1.));
#13601=DIRECTION('ref_axis',(1.,0.,0.));
#13602=DIRECTION('center_axis',(-1.,0.,0.));
#13603=DIRECTION('ref_axis',(0.,1.,0.));
#13604=DIRECTION('',(0.,-1.,0.));
#13605=DIRECTION('',(0.,0.,-1.));
#13606=DIRECTION('',(0.,1.,0.));
#13607=DIRECTION('',(0.,0.,-1.));
#13608=DIRECTION('center_axis',(0.,0.,-1.));
#13609=DIRECTION('ref_axis',(-1.,0.,0.));
#13610=DIRECTION('center_axis',(0.,0.,1.));
#13611=DIRECTION('ref_axis',(-1.,0.,0.));
#13612=DIRECTION('center_axis',(0.,0.,-1.));
#13613=DIRECTION('ref_axis',(-1.,0.,0.));
#13614=DIRECTION('',(0.,0.,-1.));
#13615=DIRECTION('center_axis',(1.,0.,0.));
#13616=DIRECTION('ref_axis',(0.,-1.,0.));
#13617=DIRECTION('',(0.,1.,0.));
#13618=DIRECTION('',(0.,-1.,0.));
#13619=DIRECTION('',(0.,0.,-1.));
#13620=DIRECTION('center_axis',(0.,0.,-1.));
#13621=DIRECTION('ref_axis',(1.,0.,0.));
#13622=DIRECTION('center_axis',(0.,0.,1.));
#13623=DIRECTION('ref_axis',(1.,0.,0.));
#13624=DIRECTION('center_axis',(0.,0.,-1.));
#13625=DIRECTION('ref_axis',(1.,0.,0.));
#13626=DIRECTION('center_axis',(0.,0.,-1.));
#13627=DIRECTION('ref_axis',(-1.,0.,0.));
#13628=DIRECTION('center_axis',(0.,0.,-1.));
#13629=DIRECTION('ref_axis',(-1.,0.,0.));
#13630=DIRECTION('',(0.,0.,-1.));
#13631=DIRECTION('center_axis',(0.,0.,1.));
#13632=DIRECTION('ref_axis',(-1.,0.,0.));
#13633=DIRECTION('center_axis',(0.,0.,-1.));
#13634=DIRECTION('ref_axis',(-1.,0.,0.));
#13635=DIRECTION('center_axis',(0.,0.,-1.));
#13636=DIRECTION('ref_axis',(-1.,0.,0.));
#13637=DIRECTION('',(0.,0.,-1.));
#13638=DIRECTION('center_axis',(0.,0.,1.));
#13639=DIRECTION('ref_axis',(-1.,0.,0.));
#13640=DIRECTION('center_axis',(0.,0.,-1.));
#13641=DIRECTION('ref_axis',(-1.,0.,0.));
#13642=DIRECTION('center_axis',(0.,0.,-1.));
#13643=DIRECTION('ref_axis',(-1.,0.,0.));
#13644=DIRECTION('',(0.,0.,-1.));
#13645=DIRECTION('center_axis',(0.,0.,1.));
#13646=DIRECTION('ref_axis',(-1.,0.,0.));
#13647=DIRECTION('center_axis',(0.,0.,-1.));
#13648=DIRECTION('ref_axis',(-1.,0.,0.));
#13649=DIRECTION('center_axis',(0.,0.,-1.));
#13650=DIRECTION('ref_axis',(-1.,0.,0.));
#13651=DIRECTION('',(0.,0.,-1.));
#13652=DIRECTION('center_axis',(0.,0.,1.));
#13653=DIRECTION('ref_axis',(-1.,0.,0.));
#13654=DIRECTION('center_axis',(0.,0.,-1.));
#13655=DIRECTION('ref_axis',(-1.,0.,0.));
#13656=DIRECTION('center_axis',(0.,0.,-1.));
#13657=DIRECTION('ref_axis',(-1.,0.,0.));
#13658=DIRECTION('',(0.,0.,-1.));
#13659=DIRECTION('center_axis',(0.,0.,1.));
#13660=DIRECTION('ref_axis',(-1.,0.,0.));
#13661=DIRECTION('center_axis',(-1.,0.,0.));
#13662=DIRECTION('ref_axis',(0.,1.,0.));
#13663=DIRECTION('',(0.,-1.,0.));
#13664=DIRECTION('',(0.,0.,-1.));
#13665=DIRECTION('',(0.,1.,0.));
#13666=DIRECTION('',(0.,0.,-1.));
#13667=DIRECTION('center_axis',(0.,0.,-1.));
#13668=DIRECTION('ref_axis',(-1.,0.,0.));
#13669=DIRECTION('center_axis',(0.,0.,1.));
#13670=DIRECTION('ref_axis',(-1.,0.,0.));
#13671=DIRECTION('center_axis',(0.,0.,-1.));
#13672=DIRECTION('ref_axis',(-1.,0.,0.));
#13673=DIRECTION('',(0.,0.,-1.));
#13674=DIRECTION('center_axis',(1.,0.,0.));
#13675=DIRECTION('ref_axis',(0.,-1.,0.));
#13676=DIRECTION('',(0.,1.,0.));
#13677=DIRECTION('',(0.,-1.,0.));
#13678=DIRECTION('',(0.,0.,-1.));
#13679=DIRECTION('center_axis',(0.,0.,-1.));
#13680=DIRECTION('ref_axis',(1.,0.,0.));
#13681=DIRECTION('center_axis',(0.,0.,1.));
#13682=DIRECTION('ref_axis',(1.,0.,0.));
#13683=DIRECTION('center_axis',(0.,0.,-1.));
#13684=DIRECTION('ref_axis',(1.,0.,0.));
#13685=DIRECTION('center_axis',(-1.,0.,0.));
#13686=DIRECTION('ref_axis',(0.,1.,0.));
#13687=DIRECTION('',(0.,-1.,0.));
#13688=DIRECTION('',(0.,0.,-1.));
#13689=DIRECTION('',(0.,1.,0.));
#13690=DIRECTION('',(0.,0.,-1.));
#13691=DIRECTION('center_axis',(0.,0.,-1.));
#13692=DIRECTION('ref_axis',(-1.,0.,0.));
#13693=DIRECTION('center_axis',(0.,0.,1.));
#13694=DIRECTION('ref_axis',(-1.,0.,0.));
#13695=DIRECTION('center_axis',(0.,0.,-1.));
#13696=DIRECTION('ref_axis',(-1.,0.,0.));
#13697=DIRECTION('',(0.,0.,-1.));
#13698=DIRECTION('center_axis',(1.,0.,0.));
#13699=DIRECTION('ref_axis',(0.,-1.,0.));
#13700=DIRECTION('',(0.,1.,0.));
#13701=DIRECTION('',(0.,-1.,0.));
#13702=DIRECTION('',(0.,0.,-1.));
#13703=DIRECTION('center_axis',(0.,0.,-1.));
#13704=DIRECTION('ref_axis',(1.,0.,0.));
#13705=DIRECTION('center_axis',(0.,0.,1.));
#13706=DIRECTION('ref_axis',(1.,0.,0.));
#13707=DIRECTION('center_axis',(0.,0.,-1.));
#13708=DIRECTION('ref_axis',(1.,0.,0.));
#13709=DIRECTION('center_axis',(0.,0.,-1.));
#13710=DIRECTION('ref_axis',(-1.,0.,0.));
#13711=DIRECTION('center_axis',(0.,0.,-1.));
#13712=DIRECTION('ref_axis',(-1.,0.,0.));
#13713=DIRECTION('',(0.,0.,-1.));
#13714=DIRECTION('center_axis',(0.,0.,1.));
#13715=DIRECTION('ref_axis',(-1.,0.,0.));
#13716=DIRECTION('center_axis',(0.,0.,-1.));
#13717=DIRECTION('ref_axis',(-1.,0.,0.));
#13718=DIRECTION('center_axis',(0.,0.,-1.));
#13719=DIRECTION('ref_axis',(-1.,0.,0.));
#13720=DIRECTION('',(0.,0.,-1.));
#13721=DIRECTION('center_axis',(0.,0.,1.));
#13722=DIRECTION('ref_axis',(-1.,0.,0.));
#13723=DIRECTION('center_axis',(0.,0.,-1.));
#13724=DIRECTION('ref_axis',(-1.,0.,0.));
#13725=DIRECTION('center_axis',(0.,0.,-1.));
#13726=DIRECTION('ref_axis',(-1.,0.,0.));
#13727=DIRECTION('',(0.,0.,-1.));
#13728=DIRECTION('center_axis',(0.,0.,1.));
#13729=DIRECTION('ref_axis',(-1.,0.,0.));
#13730=DIRECTION('center_axis',(0.,0.,-1.));
#13731=DIRECTION('ref_axis',(-1.,0.,0.));
#13732=DIRECTION('center_axis',(0.,0.,-1.));
#13733=DIRECTION('ref_axis',(-1.,0.,0.));
#13734=DIRECTION('',(0.,0.,-1.));
#13735=DIRECTION('center_axis',(0.,0.,1.));
#13736=DIRECTION('ref_axis',(-1.,0.,0.));
#13737=DIRECTION('center_axis',(0.,0.,-1.));
#13738=DIRECTION('ref_axis',(-1.,0.,0.));
#13739=DIRECTION('center_axis',(0.,0.,-1.));
#13740=DIRECTION('ref_axis',(-1.,0.,0.));
#13741=DIRECTION('',(0.,0.,-1.));
#13742=DIRECTION('center_axis',(0.,0.,1.));
#13743=DIRECTION('ref_axis',(-1.,0.,0.));
#13744=DIRECTION('center_axis',(-1.,0.,0.));
#13745=DIRECTION('ref_axis',(0.,1.,0.));
#13746=DIRECTION('',(0.,-1.,0.));
#13747=DIRECTION('',(0.,0.,-1.));
#13748=DIRECTION('',(0.,1.,0.));
#13749=DIRECTION('',(0.,0.,-1.));
#13750=DIRECTION('center_axis',(0.,0.,-1.));
#13751=DIRECTION('ref_axis',(-1.,0.,0.));
#13752=DIRECTION('center_axis',(0.,0.,1.));
#13753=DIRECTION('ref_axis',(-1.,0.,0.));
#13754=DIRECTION('center_axis',(0.,0.,-1.));
#13755=DIRECTION('ref_axis',(-1.,0.,0.));
#13756=DIRECTION('',(0.,0.,-1.));
#13757=DIRECTION('center_axis',(1.,0.,0.));
#13758=DIRECTION('ref_axis',(0.,-1.,0.));
#13759=DIRECTION('',(0.,1.,0.));
#13760=DIRECTION('',(0.,-1.,0.));
#13761=DIRECTION('',(0.,0.,-1.));
#13762=DIRECTION('center_axis',(0.,0.,-1.));
#13763=DIRECTION('ref_axis',(1.,0.,0.));
#13764=DIRECTION('center_axis',(0.,0.,1.));
#13765=DIRECTION('ref_axis',(1.,0.,0.));
#13766=DIRECTION('center_axis',(0.,0.,-1.));
#13767=DIRECTION('ref_axis',(1.,0.,0.));
#13768=DIRECTION('center_axis',(-1.,0.,0.));
#13769=DIRECTION('ref_axis',(0.,1.,0.));
#13770=DIRECTION('',(0.,-1.,0.));
#13771=DIRECTION('',(0.,0.,-1.));
#13772=DIRECTION('',(0.,1.,0.));
#13773=DIRECTION('',(0.,0.,-1.));
#13774=DIRECTION('center_axis',(0.,0.,-1.));
#13775=DIRECTION('ref_axis',(-1.,0.,0.));
#13776=DIRECTION('center_axis',(0.,0.,1.));
#13777=DIRECTION('ref_axis',(-1.,0.,0.));
#13778=DIRECTION('center_axis',(0.,0.,-1.));
#13779=DIRECTION('ref_axis',(-1.,0.,0.));
#13780=DIRECTION('',(0.,0.,-1.));
#13781=DIRECTION('center_axis',(1.,0.,0.));
#13782=DIRECTION('ref_axis',(0.,-1.,0.));
#13783=DIRECTION('',(0.,1.,0.));
#13784=DIRECTION('',(0.,-1.,0.));
#13785=DIRECTION('',(0.,0.,-1.));
#13786=DIRECTION('center_axis',(0.,0.,-1.));
#13787=DIRECTION('ref_axis',(1.,0.,0.));
#13788=DIRECTION('center_axis',(0.,0.,1.));
#13789=DIRECTION('ref_axis',(1.,0.,0.));
#13790=DIRECTION('center_axis',(0.,0.,-1.));
#13791=DIRECTION('ref_axis',(1.,0.,0.));
#13792=DIRECTION('center_axis',(0.,0.,-1.));
#13793=DIRECTION('ref_axis',(-1.,0.,0.));
#13794=DIRECTION('center_axis',(0.,0.,-1.));
#13795=DIRECTION('ref_axis',(-1.,0.,0.));
#13796=DIRECTION('',(0.,0.,-1.));
#13797=DIRECTION('center_axis',(0.,0.,1.));
#13798=DIRECTION('ref_axis',(-1.,0.,0.));
#13799=DIRECTION('center_axis',(0.,0.,-1.));
#13800=DIRECTION('ref_axis',(-1.,0.,0.));
#13801=DIRECTION('center_axis',(0.,0.,-1.));
#13802=DIRECTION('ref_axis',(-1.,0.,0.));
#13803=DIRECTION('',(0.,0.,-1.));
#13804=DIRECTION('center_axis',(0.,0.,1.));
#13805=DIRECTION('ref_axis',(-1.,0.,0.));
#13806=DIRECTION('center_axis',(0.,0.,-1.));
#13807=DIRECTION('ref_axis',(-1.,0.,0.));
#13808=DIRECTION('center_axis',(0.,0.,-1.));
#13809=DIRECTION('ref_axis',(-1.,0.,0.));
#13810=DIRECTION('',(0.,0.,-1.));
#13811=DIRECTION('center_axis',(0.,0.,1.));
#13812=DIRECTION('ref_axis',(-1.,0.,0.));
#13813=DIRECTION('center_axis',(0.,0.,-1.));
#13814=DIRECTION('ref_axis',(-1.,0.,0.));
#13815=DIRECTION('center_axis',(0.,0.,-1.));
#13816=DIRECTION('ref_axis',(-1.,0.,0.));
#13817=DIRECTION('',(0.,0.,-1.));
#13818=DIRECTION('center_axis',(0.,0.,1.));
#13819=DIRECTION('ref_axis',(-1.,0.,0.));
#13820=DIRECTION('center_axis',(0.,0.,-1.));
#13821=DIRECTION('ref_axis',(-1.,0.,0.));
#13822=DIRECTION('center_axis',(0.,0.,-1.));
#13823=DIRECTION('ref_axis',(-1.,0.,0.));
#13824=DIRECTION('',(0.,0.,-1.));
#13825=DIRECTION('center_axis',(0.,0.,1.));
#13826=DIRECTION('ref_axis',(-1.,0.,0.));
#13827=DIRECTION('center_axis',(-1.,0.,0.));
#13828=DIRECTION('ref_axis',(0.,1.,0.));
#13829=DIRECTION('',(0.,-1.,0.));
#13830=DIRECTION('',(0.,0.,-1.));
#13831=DIRECTION('',(0.,1.,0.));
#13832=DIRECTION('',(0.,0.,-1.));
#13833=DIRECTION('center_axis',(0.,0.,-1.));
#13834=DIRECTION('ref_axis',(-1.,0.,0.));
#13835=DIRECTION('center_axis',(0.,0.,1.));
#13836=DIRECTION('ref_axis',(-1.,0.,0.));
#13837=DIRECTION('center_axis',(0.,0.,-1.));
#13838=DIRECTION('ref_axis',(-1.,0.,0.));
#13839=DIRECTION('',(0.,0.,-1.));
#13840=DIRECTION('center_axis',(1.,0.,0.));
#13841=DIRECTION('ref_axis',(0.,-1.,0.));
#13842=DIRECTION('',(0.,1.,0.));
#13843=DIRECTION('',(0.,-1.,0.));
#13844=DIRECTION('',(0.,0.,-1.));
#13845=DIRECTION('center_axis',(0.,0.,-1.));
#13846=DIRECTION('ref_axis',(1.,0.,0.));
#13847=DIRECTION('center_axis',(0.,0.,1.));
#13848=DIRECTION('ref_axis',(1.,0.,0.));
#13849=DIRECTION('center_axis',(0.,0.,-1.));
#13850=DIRECTION('ref_axis',(1.,0.,0.));
#13851=DIRECTION('center_axis',(-1.,0.,0.));
#13852=DIRECTION('ref_axis',(0.,1.,0.));
#13853=DIRECTION('',(0.,-1.,0.));
#13854=DIRECTION('',(0.,0.,-1.));
#13855=DIRECTION('',(0.,1.,0.));
#13856=DIRECTION('',(0.,0.,-1.));
#13857=DIRECTION('center_axis',(0.,0.,-1.));
#13858=DIRECTION('ref_axis',(-1.,0.,0.));
#13859=DIRECTION('center_axis',(0.,0.,1.));
#13860=DIRECTION('ref_axis',(-1.,0.,0.));
#13861=DIRECTION('center_axis',(0.,0.,-1.));
#13862=DIRECTION('ref_axis',(-1.,0.,0.));
#13863=DIRECTION('',(0.,0.,-1.));
#13864=DIRECTION('center_axis',(1.,0.,0.));
#13865=DIRECTION('ref_axis',(0.,-1.,0.));
#13866=DIRECTION('',(0.,1.,0.));
#13867=DIRECTION('',(0.,-1.,0.));
#13868=DIRECTION('',(0.,0.,-1.));
#13869=DIRECTION('center_axis',(0.,0.,-1.));
#13870=DIRECTION('ref_axis',(1.,0.,0.));
#13871=DIRECTION('center_axis',(0.,0.,1.));
#13872=DIRECTION('ref_axis',(1.,0.,0.));
#13873=DIRECTION('center_axis',(0.,0.,-1.));
#13874=DIRECTION('ref_axis',(1.,0.,0.));
#13875=DIRECTION('center_axis',(0.,0.,-1.));
#13876=DIRECTION('ref_axis',(-1.,0.,0.));
#13877=DIRECTION('center_axis',(0.,0.,-1.));
#13878=DIRECTION('ref_axis',(-1.,0.,0.));
#13879=DIRECTION('',(0.,0.,-1.));
#13880=DIRECTION('center_axis',(0.,0.,1.));
#13881=DIRECTION('ref_axis',(-1.,0.,0.));
#13882=DIRECTION('center_axis',(0.,0.,-1.));
#13883=DIRECTION('ref_axis',(-1.,0.,0.));
#13884=DIRECTION('center_axis',(0.,0.,-1.));
#13885=DIRECTION('ref_axis',(-1.,0.,0.));
#13886=DIRECTION('',(0.,0.,-1.));
#13887=DIRECTION('center_axis',(0.,0.,1.));
#13888=DIRECTION('ref_axis',(-1.,0.,0.));
#13889=DIRECTION('center_axis',(0.,0.,-1.));
#13890=DIRECTION('ref_axis',(-1.,0.,0.));
#13891=DIRECTION('center_axis',(0.,0.,-1.));
#13892=DIRECTION('ref_axis',(-1.,0.,0.));
#13893=DIRECTION('',(0.,0.,-1.));
#13894=DIRECTION('center_axis',(0.,0.,1.));
#13895=DIRECTION('ref_axis',(-1.,0.,0.));
#13896=DIRECTION('center_axis',(0.,0.,-1.));
#13897=DIRECTION('ref_axis',(-1.,0.,0.));
#13898=DIRECTION('center_axis',(0.,0.,-1.));
#13899=DIRECTION('ref_axis',(-1.,0.,0.));
#13900=DIRECTION('',(0.,0.,-1.));
#13901=DIRECTION('center_axis',(0.,0.,1.));
#13902=DIRECTION('ref_axis',(-1.,0.,0.));
#13903=DIRECTION('center_axis',(0.,0.,-1.));
#13904=DIRECTION('ref_axis',(-1.,0.,0.));
#13905=DIRECTION('center_axis',(0.,0.,-1.));
#13906=DIRECTION('ref_axis',(-1.,0.,0.));
#13907=DIRECTION('',(0.,0.,-1.));
#13908=DIRECTION('center_axis',(0.,0.,1.));
#13909=DIRECTION('ref_axis',(-1.,0.,0.));
#13910=DIRECTION('center_axis',(-1.,0.,0.));
#13911=DIRECTION('ref_axis',(0.,1.,0.));
#13912=DIRECTION('',(0.,-1.,0.));
#13913=DIRECTION('',(0.,0.,-1.));
#13914=DIRECTION('',(0.,1.,0.));
#13915=DIRECTION('',(0.,0.,-1.));
#13916=DIRECTION('center_axis',(0.,0.,-1.));
#13917=DIRECTION('ref_axis',(-1.,0.,0.));
#13918=DIRECTION('center_axis',(0.,0.,1.));
#13919=DIRECTION('ref_axis',(-1.,0.,0.));
#13920=DIRECTION('center_axis',(0.,0.,-1.));
#13921=DIRECTION('ref_axis',(-1.,0.,0.));
#13922=DIRECTION('',(0.,0.,-1.));
#13923=DIRECTION('center_axis',(1.,0.,0.));
#13924=DIRECTION('ref_axis',(0.,-1.,0.));
#13925=DIRECTION('',(0.,1.,0.));
#13926=DIRECTION('',(0.,-1.,0.));
#13927=DIRECTION('',(0.,0.,-1.));
#13928=DIRECTION('center_axis',(0.,0.,-1.));
#13929=DIRECTION('ref_axis',(1.,0.,0.));
#13930=DIRECTION('center_axis',(0.,0.,1.));
#13931=DIRECTION('ref_axis',(1.,0.,0.));
#13932=DIRECTION('center_axis',(0.,0.,-1.));
#13933=DIRECTION('ref_axis',(1.,0.,0.));
#13934=DIRECTION('center_axis',(-1.,0.,0.));
#13935=DIRECTION('ref_axis',(0.,1.,0.));
#13936=DIRECTION('',(0.,-1.,0.));
#13937=DIRECTION('',(0.,0.,-1.));
#13938=DIRECTION('',(0.,1.,0.));
#13939=DIRECTION('',(0.,0.,-1.));
#13940=DIRECTION('center_axis',(0.,0.,-1.));
#13941=DIRECTION('ref_axis',(-1.,0.,0.));
#13942=DIRECTION('center_axis',(0.,0.,1.));
#13943=DIRECTION('ref_axis',(-1.,0.,0.));
#13944=DIRECTION('center_axis',(0.,0.,-1.));
#13945=DIRECTION('ref_axis',(-1.,0.,0.));
#13946=DIRECTION('',(0.,0.,-1.));
#13947=DIRECTION('center_axis',(1.,0.,0.));
#13948=DIRECTION('ref_axis',(0.,-1.,0.));
#13949=DIRECTION('',(0.,1.,0.));
#13950=DIRECTION('',(0.,-1.,0.));
#13951=DIRECTION('',(0.,0.,-1.));
#13952=DIRECTION('center_axis',(0.,0.,-1.));
#13953=DIRECTION('ref_axis',(1.,0.,0.));
#13954=DIRECTION('center_axis',(0.,0.,1.));
#13955=DIRECTION('ref_axis',(1.,0.,0.));
#13956=DIRECTION('center_axis',(0.,0.,-1.));
#13957=DIRECTION('ref_axis',(1.,0.,0.));
#13958=DIRECTION('center_axis',(0.,0.,-1.));
#13959=DIRECTION('ref_axis',(-1.,0.,0.));
#13960=DIRECTION('center_axis',(0.,0.,-1.));
#13961=DIRECTION('ref_axis',(-1.,0.,0.));
#13962=DIRECTION('',(0.,0.,-1.));
#13963=DIRECTION('center_axis',(0.,0.,1.));
#13964=DIRECTION('ref_axis',(-1.,0.,0.));
#13965=DIRECTION('center_axis',(0.,0.,-1.));
#13966=DIRECTION('ref_axis',(-1.,0.,0.));
#13967=DIRECTION('center_axis',(0.,0.,-1.));
#13968=DIRECTION('ref_axis',(-1.,0.,0.));
#13969=DIRECTION('',(0.,0.,-1.));
#13970=DIRECTION('center_axis',(0.,0.,1.));
#13971=DIRECTION('ref_axis',(-1.,0.,0.));
#13972=DIRECTION('center_axis',(0.,0.,-1.));
#13973=DIRECTION('ref_axis',(-1.,0.,0.));
#13974=DIRECTION('center_axis',(0.,0.,-1.));
#13975=DIRECTION('ref_axis',(-1.,0.,0.));
#13976=DIRECTION('',(0.,0.,-1.));
#13977=DIRECTION('center_axis',(0.,0.,1.));
#13978=DIRECTION('ref_axis',(-1.,0.,0.));
#13979=DIRECTION('center_axis',(0.,0.,-1.));
#13980=DIRECTION('ref_axis',(-1.,0.,0.));
#13981=DIRECTION('center_axis',(0.,0.,-1.));
#13982=DIRECTION('ref_axis',(-1.,0.,0.));
#13983=DIRECTION('',(0.,0.,-1.));
#13984=DIRECTION('center_axis',(0.,0.,1.));
#13985=DIRECTION('ref_axis',(-1.,0.,0.));
#13986=DIRECTION('center_axis',(0.,0.,-1.));
#13987=DIRECTION('ref_axis',(-1.,0.,0.));
#13988=DIRECTION('center_axis',(0.,0.,-1.));
#13989=DIRECTION('ref_axis',(-1.,0.,0.));
#13990=DIRECTION('',(0.,0.,-1.));
#13991=DIRECTION('center_axis',(0.,0.,1.));
#13992=DIRECTION('ref_axis',(-1.,0.,0.));
#13993=DIRECTION('center_axis',(-1.,0.,0.));
#13994=DIRECTION('ref_axis',(0.,1.,0.));
#13995=DIRECTION('',(0.,-1.,0.));
#13996=DIRECTION('',(0.,0.,-1.));
#13997=DIRECTION('',(0.,1.,0.));
#13998=DIRECTION('',(0.,0.,-1.));
#13999=DIRECTION('center_axis',(0.,0.,-1.));
#14000=DIRECTION('ref_axis',(-1.,0.,0.));
#14001=DIRECTION('center_axis',(0.,0.,1.));
#14002=DIRECTION('ref_axis',(-1.,0.,0.));
#14003=DIRECTION('center_axis',(0.,0.,-1.));
#14004=DIRECTION('ref_axis',(-1.,0.,0.));
#14005=DIRECTION('',(0.,0.,-1.));
#14006=DIRECTION('center_axis',(1.,0.,0.));
#14007=DIRECTION('ref_axis',(0.,-1.,0.));
#14008=DIRECTION('',(0.,1.,0.));
#14009=DIRECTION('',(0.,-1.,0.));
#14010=DIRECTION('',(0.,0.,-1.));
#14011=DIRECTION('center_axis',(0.,0.,-1.));
#14012=DIRECTION('ref_axis',(1.,0.,0.));
#14013=DIRECTION('center_axis',(0.,0.,1.));
#14014=DIRECTION('ref_axis',(1.,0.,0.));
#14015=DIRECTION('center_axis',(0.,0.,-1.));
#14016=DIRECTION('ref_axis',(1.,0.,0.));
#14017=DIRECTION('center_axis',(-1.,0.,0.));
#14018=DIRECTION('ref_axis',(0.,1.,0.));
#14019=DIRECTION('',(0.,-1.,0.));
#14020=DIRECTION('',(0.,0.,-1.));
#14021=DIRECTION('',(0.,1.,0.));
#14022=DIRECTION('',(0.,0.,-1.));
#14023=DIRECTION('center_axis',(0.,0.,-1.));
#14024=DIRECTION('ref_axis',(-1.,0.,0.));
#14025=DIRECTION('center_axis',(0.,0.,1.));
#14026=DIRECTION('ref_axis',(-1.,0.,0.));
#14027=DIRECTION('center_axis',(0.,0.,-1.));
#14028=DIRECTION('ref_axis',(-1.,0.,0.));
#14029=DIRECTION('',(0.,0.,-1.));
#14030=DIRECTION('center_axis',(1.,0.,0.));
#14031=DIRECTION('ref_axis',(0.,-1.,0.));
#14032=DIRECTION('',(0.,1.,0.));
#14033=DIRECTION('',(0.,-1.,0.));
#14034=DIRECTION('',(0.,0.,-1.));
#14035=DIRECTION('center_axis',(0.,0.,-1.));
#14036=DIRECTION('ref_axis',(1.,0.,0.));
#14037=DIRECTION('center_axis',(0.,0.,1.));
#14038=DIRECTION('ref_axis',(1.,0.,0.));
#14039=DIRECTION('center_axis',(0.,0.,-1.));
#14040=DIRECTION('ref_axis',(1.,0.,0.));
#14041=DIRECTION('center_axis',(0.,0.,-1.));
#14042=DIRECTION('ref_axis',(-1.,0.,0.));
#14043=DIRECTION('center_axis',(0.,0.,-1.));
#14044=DIRECTION('ref_axis',(-1.,0.,0.));
#14045=DIRECTION('',(0.,0.,-1.));
#14046=DIRECTION('center_axis',(0.,0.,1.));
#14047=DIRECTION('ref_axis',(-1.,0.,0.));
#14048=DIRECTION('center_axis',(0.,0.,-1.));
#14049=DIRECTION('ref_axis',(-1.,0.,0.));
#14050=DIRECTION('center_axis',(0.,0.,-1.));
#14051=DIRECTION('ref_axis',(-1.,0.,0.));
#14052=DIRECTION('',(0.,0.,-1.));
#14053=DIRECTION('center_axis',(0.,0.,1.));
#14054=DIRECTION('ref_axis',(-1.,0.,0.));
#14055=DIRECTION('center_axis',(0.,0.,-1.));
#14056=DIRECTION('ref_axis',(-1.,0.,0.));
#14057=DIRECTION('center_axis',(0.,0.,-1.));
#14058=DIRECTION('ref_axis',(-1.,0.,0.));
#14059=DIRECTION('',(0.,0.,-1.));
#14060=DIRECTION('center_axis',(0.,0.,1.));
#14061=DIRECTION('ref_axis',(-1.,0.,0.));
#14062=DIRECTION('center_axis',(0.,0.,-1.));
#14063=DIRECTION('ref_axis',(-1.,0.,0.));
#14064=DIRECTION('center_axis',(0.,0.,-1.));
#14065=DIRECTION('ref_axis',(-1.,0.,0.));
#14066=DIRECTION('',(0.,0.,-1.));
#14067=DIRECTION('center_axis',(0.,0.,1.));
#14068=DIRECTION('ref_axis',(-1.,0.,0.));
#14069=DIRECTION('center_axis',(0.,0.,-1.));
#14070=DIRECTION('ref_axis',(-1.,0.,0.));
#14071=DIRECTION('center_axis',(0.,0.,-1.));
#14072=DIRECTION('ref_axis',(-1.,0.,0.));
#14073=DIRECTION('',(0.,0.,-1.));
#14074=DIRECTION('center_axis',(0.,0.,1.));
#14075=DIRECTION('ref_axis',(-1.,0.,0.));
#14076=DIRECTION('center_axis',(-1.,0.,0.));
#14077=DIRECTION('ref_axis',(0.,1.,0.));
#14078=DIRECTION('',(0.,-1.,0.));
#14079=DIRECTION('',(0.,0.,-1.));
#14080=DIRECTION('',(0.,1.,0.));
#14081=DIRECTION('',(0.,0.,-1.));
#14082=DIRECTION('center_axis',(0.,0.,-1.));
#14083=DIRECTION('ref_axis',(-1.,0.,0.));
#14084=DIRECTION('center_axis',(0.,0.,1.));
#14085=DIRECTION('ref_axis',(-1.,0.,0.));
#14086=DIRECTION('center_axis',(0.,0.,-1.));
#14087=DIRECTION('ref_axis',(-1.,0.,0.));
#14088=DIRECTION('',(0.,0.,-1.));
#14089=DIRECTION('center_axis',(1.,0.,0.));
#14090=DIRECTION('ref_axis',(0.,-1.,0.));
#14091=DIRECTION('',(0.,1.,0.));
#14092=DIRECTION('',(0.,-1.,0.));
#14093=DIRECTION('',(0.,0.,-1.));
#14094=DIRECTION('center_axis',(0.,0.,-1.));
#14095=DIRECTION('ref_axis',(1.,0.,0.));
#14096=DIRECTION('center_axis',(0.,0.,1.));
#14097=DIRECTION('ref_axis',(1.,0.,0.));
#14098=DIRECTION('center_axis',(0.,0.,-1.));
#14099=DIRECTION('ref_axis',(1.,0.,0.));
#14100=DIRECTION('center_axis',(-1.,0.,0.));
#14101=DIRECTION('ref_axis',(0.,1.,0.));
#14102=DIRECTION('',(0.,-1.,0.));
#14103=DIRECTION('',(0.,0.,-1.));
#14104=DIRECTION('',(0.,1.,0.));
#14105=DIRECTION('',(0.,0.,-1.));
#14106=DIRECTION('center_axis',(0.,0.,-1.));
#14107=DIRECTION('ref_axis',(-1.,0.,0.));
#14108=DIRECTION('center_axis',(0.,0.,1.));
#14109=DIRECTION('ref_axis',(-1.,0.,0.));
#14110=DIRECTION('center_axis',(0.,0.,-1.));
#14111=DIRECTION('ref_axis',(-1.,0.,0.));
#14112=DIRECTION('',(0.,0.,-1.));
#14113=DIRECTION('center_axis',(1.,0.,0.));
#14114=DIRECTION('ref_axis',(0.,-1.,0.));
#14115=DIRECTION('',(0.,1.,0.));
#14116=DIRECTION('',(0.,-1.,0.));
#14117=DIRECTION('',(0.,0.,-1.));
#14118=DIRECTION('center_axis',(0.,0.,-1.));
#14119=DIRECTION('ref_axis',(1.,0.,0.));
#14120=DIRECTION('center_axis',(0.,0.,1.));
#14121=DIRECTION('ref_axis',(1.,0.,0.));
#14122=DIRECTION('center_axis',(0.,0.,-1.));
#14123=DIRECTION('ref_axis',(1.,0.,0.));
#14124=DIRECTION('center_axis',(0.,0.,-1.));
#14125=DIRECTION('ref_axis',(-1.,0.,0.));
#14126=DIRECTION('center_axis',(0.,0.,-1.));
#14127=DIRECTION('ref_axis',(-1.,0.,0.));
#14128=DIRECTION('',(0.,0.,-1.));
#14129=DIRECTION('center_axis',(0.,0.,1.));
#14130=DIRECTION('ref_axis',(-1.,0.,0.));
#14131=DIRECTION('center_axis',(0.,0.,-1.));
#14132=DIRECTION('ref_axis',(-1.,0.,0.));
#14133=DIRECTION('center_axis',(0.,0.,-1.));
#14134=DIRECTION('ref_axis',(-1.,0.,0.));
#14135=DIRECTION('',(0.,0.,-1.));
#14136=DIRECTION('center_axis',(0.,0.,1.));
#14137=DIRECTION('ref_axis',(-1.,0.,0.));
#14138=DIRECTION('center_axis',(0.,0.,-1.));
#14139=DIRECTION('ref_axis',(-1.,0.,0.));
#14140=DIRECTION('center_axis',(0.,0.,-1.));
#14141=DIRECTION('ref_axis',(-1.,0.,0.));
#14142=DIRECTION('',(0.,0.,-1.));
#14143=DIRECTION('center_axis',(0.,0.,1.));
#14144=DIRECTION('ref_axis',(-1.,0.,0.));
#14145=DIRECTION('center_axis',(0.,0.,-1.));
#14146=DIRECTION('ref_axis',(-1.,0.,0.));
#14147=DIRECTION('center_axis',(0.,0.,-1.));
#14148=DIRECTION('ref_axis',(-1.,0.,0.));
#14149=DIRECTION('',(0.,0.,-1.));
#14150=DIRECTION('center_axis',(0.,0.,1.));
#14151=DIRECTION('ref_axis',(-1.,0.,0.));
#14152=DIRECTION('center_axis',(0.,0.,-1.));
#14153=DIRECTION('ref_axis',(-1.,0.,0.));
#14154=DIRECTION('center_axis',(0.,0.,-1.));
#14155=DIRECTION('ref_axis',(-1.,0.,0.));
#14156=DIRECTION('',(0.,0.,-1.));
#14157=DIRECTION('center_axis',(0.,0.,1.));
#14158=DIRECTION('ref_axis',(-1.,0.,0.));
#14159=DIRECTION('center_axis',(-1.,0.,0.));
#14160=DIRECTION('ref_axis',(0.,1.,0.));
#14161=DIRECTION('',(0.,-1.,0.));
#14162=DIRECTION('',(0.,0.,-1.));
#14163=DIRECTION('',(0.,1.,0.));
#14164=DIRECTION('',(0.,0.,-1.));
#14165=DIRECTION('center_axis',(0.,0.,-1.));
#14166=DIRECTION('ref_axis',(-1.,0.,0.));
#14167=DIRECTION('center_axis',(0.,0.,1.));
#14168=DIRECTION('ref_axis',(-1.,0.,0.));
#14169=DIRECTION('center_axis',(0.,0.,-1.));
#14170=DIRECTION('ref_axis',(-1.,0.,0.));
#14171=DIRECTION('',(0.,0.,-1.));
#14172=DIRECTION('center_axis',(1.,0.,0.));
#14173=DIRECTION('ref_axis',(0.,-1.,0.));
#14174=DIRECTION('',(0.,1.,0.));
#14175=DIRECTION('',(0.,-1.,0.));
#14176=DIRECTION('',(0.,0.,-1.));
#14177=DIRECTION('center_axis',(0.,0.,-1.));
#14178=DIRECTION('ref_axis',(1.,0.,0.));
#14179=DIRECTION('center_axis',(0.,0.,1.));
#14180=DIRECTION('ref_axis',(1.,0.,0.));
#14181=DIRECTION('center_axis',(0.,0.,-1.));
#14182=DIRECTION('ref_axis',(1.,0.,0.));
#14183=DIRECTION('center_axis',(-1.,0.,0.));
#14184=DIRECTION('ref_axis',(0.,1.,0.));
#14185=DIRECTION('',(0.,-1.,0.));
#14186=DIRECTION('',(0.,0.,-1.));
#14187=DIRECTION('',(0.,1.,0.));
#14188=DIRECTION('',(0.,0.,-1.));
#14189=DIRECTION('center_axis',(0.,0.,-1.));
#14190=DIRECTION('ref_axis',(-1.,0.,0.));
#14191=DIRECTION('center_axis',(0.,0.,1.));
#14192=DIRECTION('ref_axis',(-1.,0.,0.));
#14193=DIRECTION('center_axis',(0.,0.,-1.));
#14194=DIRECTION('ref_axis',(-1.,0.,0.));
#14195=DIRECTION('',(0.,0.,-1.));
#14196=DIRECTION('center_axis',(1.,0.,0.));
#14197=DIRECTION('ref_axis',(0.,-1.,0.));
#14198=DIRECTION('',(0.,1.,0.));
#14199=DIRECTION('',(0.,-1.,0.));
#14200=DIRECTION('',(0.,0.,-1.));
#14201=DIRECTION('center_axis',(0.,0.,-1.));
#14202=DIRECTION('ref_axis',(1.,0.,0.));
#14203=DIRECTION('center_axis',(0.,0.,1.));
#14204=DIRECTION('ref_axis',(1.,0.,0.));
#14205=DIRECTION('center_axis',(0.,0.,-1.));
#14206=DIRECTION('ref_axis',(1.,0.,0.));
#14207=DIRECTION('center_axis',(0.,0.,-1.));
#14208=DIRECTION('ref_axis',(-1.,0.,0.));
#14209=DIRECTION('center_axis',(0.,0.,-1.));
#14210=DIRECTION('ref_axis',(-1.,0.,0.));
#14211=DIRECTION('',(0.,0.,-1.));
#14212=DIRECTION('center_axis',(0.,0.,1.));
#14213=DIRECTION('ref_axis',(-1.,0.,0.));
#14214=DIRECTION('center_axis',(0.,0.,-1.));
#14215=DIRECTION('ref_axis',(-1.,0.,0.));
#14216=DIRECTION('center_axis',(0.,0.,-1.));
#14217=DIRECTION('ref_axis',(-1.,0.,0.));
#14218=DIRECTION('',(0.,0.,-1.));
#14219=DIRECTION('center_axis',(0.,0.,1.));
#14220=DIRECTION('ref_axis',(-1.,0.,0.));
#14221=DIRECTION('center_axis',(-1.,0.,0.));
#14222=DIRECTION('ref_axis',(0.,1.,0.));
#14223=DIRECTION('',(0.,-1.,0.));
#14224=DIRECTION('',(0.,0.,-1.));
#14225=DIRECTION('',(0.,1.,0.));
#14226=DIRECTION('',(0.,0.,-1.));
#14227=DIRECTION('center_axis',(0.,0.,-1.));
#14228=DIRECTION('ref_axis',(-1.,0.,0.));
#14229=DIRECTION('center_axis',(0.,0.,1.));
#14230=DIRECTION('ref_axis',(-1.,0.,0.));
#14231=DIRECTION('center_axis',(0.,0.,-1.));
#14232=DIRECTION('ref_axis',(-1.,0.,0.));
#14233=DIRECTION('',(0.,0.,-1.));
#14234=DIRECTION('center_axis',(1.,0.,0.));
#14235=DIRECTION('ref_axis',(0.,-1.,0.));
#14236=DIRECTION('',(0.,1.,0.));
#14237=DIRECTION('',(0.,-1.,0.));
#14238=DIRECTION('',(0.,0.,-1.));
#14239=DIRECTION('center_axis',(0.,0.,-1.));
#14240=DIRECTION('ref_axis',(1.,0.,0.));
#14241=DIRECTION('center_axis',(0.,0.,1.));
#14242=DIRECTION('ref_axis',(1.,0.,0.));
#14243=DIRECTION('center_axis',(0.,0.,-1.));
#14244=DIRECTION('ref_axis',(1.,0.,0.));
#14245=DIRECTION('center_axis',(-1.,0.,0.));
#14246=DIRECTION('ref_axis',(0.,1.,0.));
#14247=DIRECTION('',(0.,-1.,0.));
#14248=DIRECTION('',(0.,0.,-1.));
#14249=DIRECTION('',(0.,1.,0.));
#14250=DIRECTION('',(0.,0.,-1.));
#14251=DIRECTION('center_axis',(0.,0.,-1.));
#14252=DIRECTION('ref_axis',(-1.,0.,0.));
#14253=DIRECTION('center_axis',(0.,0.,1.));
#14254=DIRECTION('ref_axis',(-1.,0.,0.));
#14255=DIRECTION('center_axis',(0.,0.,-1.));
#14256=DIRECTION('ref_axis',(-1.,0.,0.));
#14257=DIRECTION('',(0.,0.,-1.));
#14258=DIRECTION('center_axis',(1.,0.,0.));
#14259=DIRECTION('ref_axis',(0.,-1.,0.));
#14260=DIRECTION('',(0.,1.,0.));
#14261=DIRECTION('',(0.,-1.,0.));
#14262=DIRECTION('',(0.,0.,-1.));
#14263=DIRECTION('center_axis',(0.,0.,-1.));
#14264=DIRECTION('ref_axis',(1.,0.,0.));
#14265=DIRECTION('center_axis',(0.,0.,1.));
#14266=DIRECTION('ref_axis',(1.,0.,0.));
#14267=DIRECTION('center_axis',(0.,0.,-1.));
#14268=DIRECTION('ref_axis',(1.,0.,0.));
#14269=DIRECTION('center_axis',(0.,0.,-1.));
#14270=DIRECTION('ref_axis',(-1.,0.,0.));
#14271=DIRECTION('center_axis',(0.,0.,-1.));
#14272=DIRECTION('ref_axis',(-1.,0.,0.));
#14273=DIRECTION('',(0.,0.,-1.));
#14274=DIRECTION('center_axis',(0.,0.,1.));
#14275=DIRECTION('ref_axis',(-1.,0.,0.));
#14276=DIRECTION('center_axis',(0.,0.,-1.));
#14277=DIRECTION('ref_axis',(-1.,0.,0.));
#14278=DIRECTION('center_axis',(0.,0.,-1.));
#14279=DIRECTION('ref_axis',(-1.,0.,0.));
#14280=DIRECTION('',(0.,0.,-1.));
#14281=DIRECTION('center_axis',(0.,0.,1.));
#14282=DIRECTION('ref_axis',(-1.,0.,0.));
#14283=DIRECTION('center_axis',(0.,0.,-1.));
#14284=DIRECTION('ref_axis',(-1.,0.,0.));
#14285=DIRECTION('center_axis',(0.,0.,-1.));
#14286=DIRECTION('ref_axis',(-1.,0.,0.));
#14287=DIRECTION('',(0.,0.,-1.));
#14288=DIRECTION('center_axis',(0.,0.,1.));
#14289=DIRECTION('ref_axis',(-1.,0.,0.));
#14290=DIRECTION('center_axis',(1.,0.,0.));
#14291=DIRECTION('ref_axis',(0.,-0.707106781186547,0.707106781186548));
#14292=DIRECTION('center_axis',(-1.,0.,0.));
#14293=DIRECTION('ref_axis',(0.,-0.707106781186547,0.707106781186548));
#14294=DIRECTION('',(1.,0.,0.));
#14295=DIRECTION('center_axis',(1.,0.,0.));
#14296=DIRECTION('ref_axis',(0.,-0.707106781186547,0.707106781186548));
#14297=DIRECTION('',(-1.,0.,0.));
#14298=DIRECTION('center_axis',(0.,0.,-1.));
#14299=DIRECTION('ref_axis',(-1.,0.,0.));
#14300=DIRECTION('',(0.,1.,0.));
#14301=DIRECTION('',(-1.,0.,0.));
#14302=DIRECTION('',(0.,1.,0.));
#14303=DIRECTION('center_axis',(1.,0.,0.));
#14304=DIRECTION('ref_axis',(0.,0.70710678118654,0.707106781186555));
#14305=DIRECTION('center_axis',(-1.,0.,0.));
#14306=DIRECTION('ref_axis',(0.,0.70710678118654,0.707106781186555));
#14307=DIRECTION('',(1.,0.,0.));
#14308=DIRECTION('center_axis',(1.,0.,0.));
#14309=DIRECTION('ref_axis',(0.,0.70710678118654,0.707106781186555));
#14310=DIRECTION('center_axis',(0.,1.,0.));
#14311=DIRECTION('ref_axis',(1.,0.,0.));
#14312=DIRECTION('',(0.,0.,-1.));
#14313=DIRECTION('',(1.,0.,0.));
#14314=DIRECTION('',(0.,0.,1.));
#14315=DIRECTION('center_axis',(0.,-1.,0.));
#14316=DIRECTION('ref_axis',(1.,0.,0.));
#14317=DIRECTION('center_axis',(0.,-1.,0.));
#14318=DIRECTION('ref_axis',(1.,0.,0.));
#14319=DIRECTION('center_axis',(0.,-1.,0.));
#14320=DIRECTION('ref_axis',(1.,0.,0.));
#14321=DIRECTION('center_axis',(0.,-1.,0.));
#14322=DIRECTION('ref_axis',(1.,0.,0.));
#14323=DIRECTION('center_axis',(0.,-1.,0.));
#14324=DIRECTION('ref_axis',(1.,0.,0.));
#14325=DIRECTION('center_axis',(0.,-1.,0.));
#14326=DIRECTION('ref_axis',(1.,0.,0.));
#14327=DIRECTION('center_axis',(0.,-1.,0.));
#14328=DIRECTION('ref_axis',(1.,0.,0.));
#14329=DIRECTION('center_axis',(0.,-1.,0.));
#14330=DIRECTION('ref_axis',(1.,0.,0.));
#14331=DIRECTION('center_axis',(0.,-1.,0.));
#14332=DIRECTION('ref_axis',(1.,0.,0.));
#14333=DIRECTION('center_axis',(0.,-1.,0.));
#14334=DIRECTION('ref_axis',(1.,0.,0.));
#14335=DIRECTION('center_axis',(0.,-1.,0.));
#14336=DIRECTION('ref_axis',(1.,0.,0.));
#14337=DIRECTION('center_axis',(0.,-1.,0.));
#14338=DIRECTION('ref_axis',(1.,0.,0.));
#14339=DIRECTION('center_axis',(0.,-1.,0.));
#14340=DIRECTION('ref_axis',(1.,0.,0.));
#14341=DIRECTION('center_axis',(0.,-1.,0.));
#14342=DIRECTION('ref_axis',(1.,0.,0.));
#14343=DIRECTION('center_axis',(0.,-1.,0.));
#14344=DIRECTION('ref_axis',(1.,0.,0.));
#14345=DIRECTION('center_axis',(0.,-1.,0.));
#14346=DIRECTION('ref_axis',(1.,0.,0.));
#14347=DIRECTION('center_axis',(0.,-1.,0.));
#14348=DIRECTION('ref_axis',(1.,0.,0.));
#14349=DIRECTION('center_axis',(0.,-1.,0.));
#14350=DIRECTION('ref_axis',(1.,0.,0.));
#14351=DIRECTION('center_axis',(0.,-1.,0.));
#14352=DIRECTION('ref_axis',(1.,0.,0.));
#14353=DIRECTION('center_axis',(0.,-1.,0.));
#14354=DIRECTION('ref_axis',(1.,0.,0.));
#14355=DIRECTION('center_axis',(0.,-1.,0.));
#14356=DIRECTION('ref_axis',(1.,0.,0.));
#14357=DIRECTION('center_axis',(0.,-1.,0.));
#14358=DIRECTION('ref_axis',(1.,0.,0.));
#14359=DIRECTION('center_axis',(0.,-1.,0.));
#14360=DIRECTION('ref_axis',(1.,0.,0.));
#14361=DIRECTION('center_axis',(0.,-1.,0.));
#14362=DIRECTION('ref_axis',(1.,0.,0.));
#14363=DIRECTION('center_axis',(0.,-1.,0.));
#14364=DIRECTION('ref_axis',(1.,0.,0.));
#14365=DIRECTION('center_axis',(0.,-1.,0.));
#14366=DIRECTION('ref_axis',(1.,0.,0.));
#14367=DIRECTION('center_axis',(0.,-1.,0.));
#14368=DIRECTION('ref_axis',(1.,0.,0.));
#14369=DIRECTION('center_axis',(0.,-1.,0.));
#14370=DIRECTION('ref_axis',(1.,0.,0.));
#14371=DIRECTION('center_axis',(0.,-1.,0.));
#14372=DIRECTION('ref_axis',(1.,0.,0.));
#14373=DIRECTION('center_axis',(0.,-1.,0.));
#14374=DIRECTION('ref_axis',(1.,0.,0.));
#14375=DIRECTION('center_axis',(0.,-1.,0.));
#14376=DIRECTION('ref_axis',(1.,0.,0.));
#14377=DIRECTION('center_axis',(0.,-1.,0.));
#14378=DIRECTION('ref_axis',(1.,0.,0.));
#14379=DIRECTION('center_axis',(0.,-1.,0.));
#14380=DIRECTION('ref_axis',(1.,0.,0.));
#14381=DIRECTION('center_axis',(0.,-1.,0.));
#14382=DIRECTION('ref_axis',(1.,0.,0.));
#14383=DIRECTION('center_axis',(0.,-1.,0.));
#14384=DIRECTION('ref_axis',(1.,0.,0.));
#14385=DIRECTION('center_axis',(0.,-1.,0.));
#14386=DIRECTION('ref_axis',(1.,0.,0.));
#14387=DIRECTION('center_axis',(0.,-1.,0.));
#14388=DIRECTION('ref_axis',(1.,0.,0.));
#14389=DIRECTION('center_axis',(0.,-1.,0.));
#14390=DIRECTION('ref_axis',(1.,0.,0.));
#14391=DIRECTION('center_axis',(0.,-1.,0.));
#14392=DIRECTION('ref_axis',(1.,0.,0.));
#14393=DIRECTION('center_axis',(0.,-1.,0.));
#14394=DIRECTION('ref_axis',(1.,0.,0.));
#14395=DIRECTION('center_axis',(0.,-1.,0.));
#14396=DIRECTION('ref_axis',(1.,0.,0.));
#14397=DIRECTION('center_axis',(0.,-1.,0.));
#14398=DIRECTION('ref_axis',(1.,0.,0.));
#14399=DIRECTION('center_axis',(0.,-1.,0.));
#14400=DIRECTION('ref_axis',(1.,0.,0.));
#14401=DIRECTION('center_axis',(0.,-1.,0.));
#14402=DIRECTION('ref_axis',(1.,0.,0.));
#14403=DIRECTION('center_axis',(0.,-1.,0.));
#14404=DIRECTION('ref_axis',(1.,0.,0.));
#14405=DIRECTION('center_axis',(0.,-1.,0.));
#14406=DIRECTION('ref_axis',(1.,0.,0.));
#14407=DIRECTION('center_axis',(0.,-1.,0.));
#14408=DIRECTION('ref_axis',(1.,0.,0.));
#14409=DIRECTION('center_axis',(1.,0.,0.));
#14410=DIRECTION('ref_axis',(0.,0.70710678118655,0.707106781186545));
#14411=DIRECTION('center_axis',(-1.,0.,0.));
#14412=DIRECTION('ref_axis',(0.,0.70710678118655,0.707106781186545));
#14413=DIRECTION('',(-1.,0.,0.));
#14414=DIRECTION('center_axis',(1.,0.,0.));
#14415=DIRECTION('ref_axis',(0.,0.70710678118655,0.707106781186545));
#14416=DIRECTION('',(1.,0.,0.));
#14417=DIRECTION('center_axis',(0.,0.,1.));
#14418=DIRECTION('ref_axis',(1.,0.,0.));
#14419=DIRECTION('',(0.,1.,0.));
#14420=DIRECTION('',(-1.,0.,0.));
#14421=DIRECTION('',(0.,1.,0.));
#14422=DIRECTION('center_axis',(-1.,0.,0.));
#14423=DIRECTION('ref_axis',(0.,0.,1.));
#14424=DIRECTION('',(0.,0.,1.));
#14425=DIRECTION('',(0.,1.,0.));
#14426=DIRECTION('',(0.,0.,1.));
#14427=DIRECTION('',(0.,1.,0.));
#14428=DIRECTION('',(0.,0.,-1.));
#14429=DIRECTION('center_axis',(1.,0.,0.));
#14430=DIRECTION('ref_axis',(0.,-0.707106781186548,0.707106781186547));
#14431=DIRECTION('center_axis',(1.,0.,0.));
#14432=DIRECTION('ref_axis',(0.,-0.707106781186548,0.707106781186547));
#14433=DIRECTION('center_axis',(-1.,0.,0.));
#14434=DIRECTION('ref_axis',(0.,-0.707106781186548,0.707106781186547));
#14435=DIRECTION('',(1.,0.,0.));
#14436=DIRECTION('center_axis',(0.,1.,0.));
#14437=DIRECTION('ref_axis',(1.,0.,0.));
#14438=DIRECTION('center_axis',(0.,-1.,0.));
#14439=DIRECTION('ref_axis',(1.,0.,0.));
#14440=DIRECTION('',(0.,-1.,0.));
#14441=DIRECTION('center_axis',(0.,1.,0.));
#14442=DIRECTION('ref_axis',(1.,0.,0.));
#14443=DIRECTION('center_axis',(0.,-1.,0.));
#14444=DIRECTION('ref_axis',(1.,0.,0.));
#14445=DIRECTION('',(0.,-1.,0.));
#14446=DIRECTION('center_axis',(0.,1.,0.));
#14447=DIRECTION('ref_axis',(1.,0.,0.));
#14448=DIRECTION('center_axis',(0.,-1.,0.));
#14449=DIRECTION('ref_axis',(1.,0.,0.));
#14450=DIRECTION('',(0.,-1.,0.));
#14451=DIRECTION('center_axis',(0.,1.,0.));
#14452=DIRECTION('ref_axis',(1.,0.,0.));
#14453=DIRECTION('center_axis',(0.,-1.,0.));
#14454=DIRECTION('ref_axis',(1.,0.,0.));
#14455=DIRECTION('',(0.,-1.,0.));
#14456=DIRECTION('center_axis',(0.,1.,0.));
#14457=DIRECTION('ref_axis',(1.,0.,0.));
#14458=DIRECTION('center_axis',(0.,-1.,0.));
#14459=DIRECTION('ref_axis',(1.,0.,0.));
#14460=DIRECTION('',(0.,-1.,0.));
#14461=DIRECTION('center_axis',(0.,1.,0.));
#14462=DIRECTION('ref_axis',(1.,0.,0.));
#14463=DIRECTION('center_axis',(0.,-1.,0.));
#14464=DIRECTION('ref_axis',(1.,0.,0.));
#14465=DIRECTION('',(0.,-1.,0.));
#14466=DIRECTION('center_axis',(0.,1.,0.));
#14467=DIRECTION('ref_axis',(1.,0.,0.));
#14468=DIRECTION('center_axis',(0.,-1.,0.));
#14469=DIRECTION('ref_axis',(1.,0.,0.));
#14470=DIRECTION('',(0.,-1.,0.));
#14471=DIRECTION('center_axis',(0.,1.,0.));
#14472=DIRECTION('ref_axis',(1.,0.,0.));
#14473=DIRECTION('center_axis',(0.,-1.,0.));
#14474=DIRECTION('ref_axis',(1.,0.,0.));
#14475=DIRECTION('',(0.,-1.,0.));
#14476=DIRECTION('center_axis',(0.,1.,0.));
#14477=DIRECTION('ref_axis',(1.,0.,0.));
#14478=DIRECTION('center_axis',(0.,-1.,0.));
#14479=DIRECTION('ref_axis',(1.,0.,0.));
#14480=DIRECTION('',(0.,-1.,0.));
#14481=DIRECTION('center_axis',(0.,1.,0.));
#14482=DIRECTION('ref_axis',(1.,0.,0.));
#14483=DIRECTION('center_axis',(0.,-1.,0.));
#14484=DIRECTION('ref_axis',(1.,0.,0.));
#14485=DIRECTION('',(0.,-1.,0.));
#14486=DIRECTION('center_axis',(0.,1.,0.));
#14487=DIRECTION('ref_axis',(1.,0.,0.));
#14488=DIRECTION('center_axis',(0.,-1.,0.));
#14489=DIRECTION('ref_axis',(1.,0.,0.));
#14490=DIRECTION('',(0.,-1.,0.));
#14491=DIRECTION('center_axis',(0.,1.,0.));
#14492=DIRECTION('ref_axis',(1.,0.,0.));
#14493=DIRECTION('center_axis',(0.,-1.,0.));
#14494=DIRECTION('ref_axis',(1.,0.,0.));
#14495=DIRECTION('',(0.,-1.,0.));
#14496=DIRECTION('center_axis',(0.,1.,0.));
#14497=DIRECTION('ref_axis',(1.,0.,0.));
#14498=DIRECTION('center_axis',(0.,-1.,0.));
#14499=DIRECTION('ref_axis',(1.,0.,0.));
#14500=DIRECTION('',(0.,-1.,0.));
#14501=DIRECTION('center_axis',(0.,1.,0.));
#14502=DIRECTION('ref_axis',(1.,0.,0.));
#14503=DIRECTION('center_axis',(0.,-1.,0.));
#14504=DIRECTION('ref_axis',(1.,0.,0.));
#14505=DIRECTION('',(0.,-1.,0.));
#14506=DIRECTION('center_axis',(0.,1.,0.));
#14507=DIRECTION('ref_axis',(1.,0.,0.));
#14508=DIRECTION('center_axis',(0.,-1.,0.));
#14509=DIRECTION('ref_axis',(1.,0.,0.));
#14510=DIRECTION('',(0.,-1.,0.));
#14511=DIRECTION('center_axis',(0.,1.,0.));
#14512=DIRECTION('ref_axis',(1.,0.,0.));
#14513=DIRECTION('center_axis',(0.,-1.,0.));
#14514=DIRECTION('ref_axis',(1.,0.,0.));
#14515=DIRECTION('',(0.,-1.,0.));
#14516=DIRECTION('center_axis',(0.,1.,0.));
#14517=DIRECTION('ref_axis',(1.,0.,0.));
#14518=DIRECTION('center_axis',(0.,-1.,0.));
#14519=DIRECTION('ref_axis',(1.,0.,0.));
#14520=DIRECTION('',(0.,-1.,0.));
#14521=DIRECTION('center_axis',(0.,1.,0.));
#14522=DIRECTION('ref_axis',(1.,0.,0.));
#14523=DIRECTION('center_axis',(0.,-1.,0.));
#14524=DIRECTION('ref_axis',(1.,0.,0.));
#14525=DIRECTION('',(0.,-1.,0.));
#14526=DIRECTION('center_axis',(0.,1.,0.));
#14527=DIRECTION('ref_axis',(1.,0.,0.));
#14528=DIRECTION('center_axis',(0.,-1.,0.));
#14529=DIRECTION('ref_axis',(1.,0.,0.));
#14530=DIRECTION('',(0.,-1.,0.));
#14531=DIRECTION('center_axis',(0.,1.,0.));
#14532=DIRECTION('ref_axis',(1.,0.,0.));
#14533=DIRECTION('center_axis',(0.,-1.,0.));
#14534=DIRECTION('ref_axis',(1.,0.,0.));
#14535=DIRECTION('',(0.,-1.,0.));
#14536=DIRECTION('center_axis',(0.,1.,0.));
#14537=DIRECTION('ref_axis',(1.,0.,0.));
#14538=DIRECTION('center_axis',(0.,-1.,0.));
#14539=DIRECTION('ref_axis',(1.,0.,0.));
#14540=DIRECTION('',(0.,-1.,0.));
#14541=DIRECTION('center_axis',(0.,1.,0.));
#14542=DIRECTION('ref_axis',(1.,0.,0.));
#14543=DIRECTION('center_axis',(0.,-1.,0.));
#14544=DIRECTION('ref_axis',(1.,0.,0.));
#14545=DIRECTION('',(0.,-1.,0.));
#14546=DIRECTION('center_axis',(0.,1.,0.));
#14547=DIRECTION('ref_axis',(1.,0.,0.));
#14548=DIRECTION('center_axis',(0.,-1.,0.));
#14549=DIRECTION('ref_axis',(1.,0.,0.));
#14550=DIRECTION('',(0.,-1.,0.));
#14551=DIRECTION('center_axis',(0.,1.,0.));
#14552=DIRECTION('ref_axis',(1.,0.,0.));
#14553=DIRECTION('center_axis',(0.,-1.,0.));
#14554=DIRECTION('ref_axis',(1.,0.,0.));
#14555=DIRECTION('',(0.,-1.,0.));
#14556=DIRECTION('center_axis',(0.,1.,0.));
#14557=DIRECTION('ref_axis',(1.,0.,0.));
#14558=DIRECTION('center_axis',(0.,-1.,0.));
#14559=DIRECTION('ref_axis',(1.,0.,0.));
#14560=DIRECTION('',(0.,-1.,0.));
#14561=DIRECTION('center_axis',(0.,1.,0.));
#14562=DIRECTION('ref_axis',(1.,0.,0.));
#14563=DIRECTION('center_axis',(0.,-1.,0.));
#14564=DIRECTION('ref_axis',(1.,0.,0.));
#14565=DIRECTION('',(0.,-1.,0.));
#14566=DIRECTION('center_axis',(0.,1.,0.));
#14567=DIRECTION('ref_axis',(1.,0.,0.));
#14568=DIRECTION('center_axis',(0.,-1.,0.));
#14569=DIRECTION('ref_axis',(1.,0.,0.));
#14570=DIRECTION('',(0.,-1.,0.));
#14571=DIRECTION('center_axis',(0.,1.,0.));
#14572=DIRECTION('ref_axis',(1.,0.,0.));
#14573=DIRECTION('center_axis',(0.,-1.,0.));
#14574=DIRECTION('ref_axis',(1.,0.,0.));
#14575=DIRECTION('',(0.,-1.,0.));
#14576=DIRECTION('center_axis',(0.,1.,0.));
#14577=DIRECTION('ref_axis',(1.,0.,0.));
#14578=DIRECTION('center_axis',(0.,-1.,0.));
#14579=DIRECTION('ref_axis',(1.,0.,0.));
#14580=DIRECTION('',(0.,-1.,0.));
#14581=DIRECTION('center_axis',(0.,1.,0.));
#14582=DIRECTION('ref_axis',(1.,0.,0.));
#14583=DIRECTION('center_axis',(0.,-1.,0.));
#14584=DIRECTION('ref_axis',(1.,0.,0.));
#14585=DIRECTION('',(0.,-1.,0.));
#14586=DIRECTION('center_axis',(0.,1.,0.));
#14587=DIRECTION('ref_axis',(1.,0.,0.));
#14588=DIRECTION('center_axis',(0.,-1.,0.));
#14589=DIRECTION('ref_axis',(1.,0.,0.));
#14590=DIRECTION('',(0.,-1.,0.));
#14591=DIRECTION('center_axis',(0.,1.,0.));
#14592=DIRECTION('ref_axis',(1.,0.,0.));
#14593=DIRECTION('center_axis',(0.,-1.,0.));
#14594=DIRECTION('ref_axis',(1.,0.,0.));
#14595=DIRECTION('',(0.,-1.,0.));
#14596=DIRECTION('center_axis',(0.,1.,0.));
#14597=DIRECTION('ref_axis',(1.,0.,0.));
#14598=DIRECTION('center_axis',(0.,-1.,0.));
#14599=DIRECTION('ref_axis',(1.,0.,0.));
#14600=DIRECTION('',(0.,-1.,0.));
#14601=DIRECTION('center_axis',(0.,1.,0.));
#14602=DIRECTION('ref_axis',(1.,0.,0.));
#14603=DIRECTION('center_axis',(0.,-1.,0.));
#14604=DIRECTION('ref_axis',(1.,0.,0.));
#14605=DIRECTION('',(0.,-1.,0.));
#14606=DIRECTION('center_axis',(0.,1.,0.));
#14607=DIRECTION('ref_axis',(1.,0.,0.));
#14608=DIRECTION('center_axis',(0.,-1.,0.));
#14609=DIRECTION('ref_axis',(1.,0.,0.));
#14610=DIRECTION('',(0.,-1.,0.));
#14611=DIRECTION('center_axis',(0.,1.,0.));
#14612=DIRECTION('ref_axis',(1.,0.,0.));
#14613=DIRECTION('center_axis',(0.,-1.,0.));
#14614=DIRECTION('ref_axis',(1.,0.,0.));
#14615=DIRECTION('',(0.,-1.,0.));
#14616=DIRECTION('center_axis',(0.,1.,0.));
#14617=DIRECTION('ref_axis',(1.,0.,0.));
#14618=DIRECTION('center_axis',(0.,-1.,0.));
#14619=DIRECTION('ref_axis',(1.,0.,0.));
#14620=DIRECTION('',(0.,-1.,0.));
#14621=DIRECTION('center_axis',(0.,1.,0.));
#14622=DIRECTION('ref_axis',(1.,0.,0.));
#14623=DIRECTION('center_axis',(0.,-1.,0.));
#14624=DIRECTION('ref_axis',(1.,0.,0.));
#14625=DIRECTION('',(0.,-1.,0.));
#14626=DIRECTION('center_axis',(0.,1.,0.));
#14627=DIRECTION('ref_axis',(1.,0.,0.));
#14628=DIRECTION('center_axis',(0.,-1.,0.));
#14629=DIRECTION('ref_axis',(1.,0.,0.));
#14630=DIRECTION('',(0.,-1.,0.));
#14631=DIRECTION('center_axis',(0.,1.,0.));
#14632=DIRECTION('ref_axis',(1.,0.,0.));
#14633=DIRECTION('center_axis',(0.,-1.,0.));
#14634=DIRECTION('ref_axis',(1.,0.,0.));
#14635=DIRECTION('',(0.,-1.,0.));
#14636=DIRECTION('center_axis',(0.,1.,0.));
#14637=DIRECTION('ref_axis',(1.,0.,0.));
#14638=DIRECTION('center_axis',(0.,-1.,0.));
#14639=DIRECTION('ref_axis',(1.,0.,0.));
#14640=DIRECTION('',(0.,-1.,0.));
#14641=DIRECTION('center_axis',(0.,1.,0.));
#14642=DIRECTION('ref_axis',(1.,0.,0.));
#14643=DIRECTION('center_axis',(0.,-1.,0.));
#14644=DIRECTION('ref_axis',(1.,0.,0.));
#14645=DIRECTION('',(0.,-1.,0.));
#14646=DIRECTION('center_axis',(0.,1.,0.));
#14647=DIRECTION('ref_axis',(1.,0.,0.));
#14648=DIRECTION('center_axis',(0.,-1.,0.));
#14649=DIRECTION('ref_axis',(1.,0.,0.));
#14650=DIRECTION('',(0.,-1.,0.));
#14651=DIRECTION('center_axis',(0.,1.,0.));
#14652=DIRECTION('ref_axis',(1.,0.,0.));
#14653=DIRECTION('center_axis',(0.,-1.,0.));
#14654=DIRECTION('ref_axis',(1.,0.,0.));
#14655=DIRECTION('',(0.,-1.,0.));
#14656=DIRECTION('center_axis',(0.,1.,0.));
#14657=DIRECTION('ref_axis',(1.,0.,0.));
#14658=DIRECTION('center_axis',(0.,-1.,0.));
#14659=DIRECTION('ref_axis',(1.,0.,0.));
#14660=DIRECTION('',(0.,-1.,0.));
#14661=DIRECTION('center_axis',(0.,1.,0.));
#14662=DIRECTION('ref_axis',(1.,0.,0.));
#14663=DIRECTION('center_axis',(0.,-1.,0.));
#14664=DIRECTION('ref_axis',(1.,0.,0.));
#14665=DIRECTION('',(0.,-1.,0.));
#14666=DIRECTION('center_axis',(0.,1.,0.));
#14667=DIRECTION('ref_axis',(1.,0.,0.));
#14668=DIRECTION('center_axis',(0.,-1.,0.));
#14669=DIRECTION('ref_axis',(1.,0.,0.));
#14670=DIRECTION('',(0.,-1.,0.));
#14671=DIRECTION('center_axis',(0.,0.,-1.));
#14672=DIRECTION('ref_axis',(-1.,0.,0.));
#14673=DIRECTION('',(-1.,0.,0.));
#14674=DIRECTION('',(0.,1.,0.));
#14675=DIRECTION('center_axis',(0.,1.,0.));
#14676=DIRECTION('ref_axis',(0.,0.,1.));
#14677=DIRECTION('',(0.,0.,-1.));
#14678=DIRECTION('center_axis',(0.,1.,0.));
#14679=DIRECTION('ref_axis',(1.,0.,0.));
#14680=DIRECTION('center_axis',(0.,-1.,0.));
#14681=DIRECTION('ref_axis',(1.,0.,0.));
#14682=DIRECTION('',(0.,-1.,0.));
#14683=DIRECTION('center_axis',(0.,-1.,0.));
#14684=DIRECTION('ref_axis',(1.,0.,0.));
#14685=DIRECTION('center_axis',(0.,1.,0.));
#14686=DIRECTION('ref_axis',(1.,0.,0.));
#14687=DIRECTION('center_axis',(0.,-1.,0.));
#14688=DIRECTION('ref_axis',(1.,0.,0.));
#14689=DIRECTION('',(0.,-1.,0.));
#14690=DIRECTION('center_axis',(0.,-1.,0.));
#14691=DIRECTION('ref_axis',(1.,0.,0.));
#14692=DIRECTION('center_axis',(0.,1.,0.));
#14693=DIRECTION('ref_axis',(1.,0.,0.));
#14694=DIRECTION('center_axis',(0.,-1.,0.));
#14695=DIRECTION('ref_axis',(1.,0.,0.));
#14696=DIRECTION('',(0.,-1.,0.));
#14697=DIRECTION('center_axis',(0.,-1.,0.));
#14698=DIRECTION('ref_axis',(1.,0.,0.));
#14699=DIRECTION('center_axis',(0.,1.,0.));
#14700=DIRECTION('ref_axis',(1.,0.,0.));
#14701=DIRECTION('center_axis',(0.,-1.,0.));
#14702=DIRECTION('ref_axis',(1.,0.,0.));
#14703=DIRECTION('',(0.,-1.,0.));
#14704=DIRECTION('center_axis',(0.,-1.,0.));
#14705=DIRECTION('ref_axis',(1.,0.,0.));
#14706=DIRECTION('center_axis',(0.,1.,0.));
#14707=DIRECTION('ref_axis',(1.,0.,0.));
#14708=DIRECTION('center_axis',(0.,-1.,0.));
#14709=DIRECTION('ref_axis',(1.,0.,0.));
#14710=DIRECTION('',(0.,-1.,0.));
#14711=DIRECTION('center_axis',(0.,-1.,0.));
#14712=DIRECTION('ref_axis',(1.,0.,0.));
#14713=DIRECTION('center_axis',(0.,1.,0.));
#14714=DIRECTION('ref_axis',(1.,0.,0.));
#14715=DIRECTION('center_axis',(0.,-1.,0.));
#14716=DIRECTION('ref_axis',(1.,0.,0.));
#14717=DIRECTION('',(0.,-1.,0.));
#14718=DIRECTION('center_axis',(0.,-1.,0.));
#14719=DIRECTION('ref_axis',(1.,0.,0.));
#14720=DIRECTION('center_axis',(0.,1.,0.));
#14721=DIRECTION('ref_axis',(1.,0.,0.));
#14722=DIRECTION('center_axis',(0.,-1.,0.));
#14723=DIRECTION('ref_axis',(1.,0.,0.));
#14724=DIRECTION('',(0.,-1.,0.));
#14725=DIRECTION('center_axis',(0.,-1.,0.));
#14726=DIRECTION('ref_axis',(1.,0.,0.));
#14727=DIRECTION('center_axis',(0.,1.,0.));
#14728=DIRECTION('ref_axis',(1.,0.,0.));
#14729=DIRECTION('center_axis',(0.,-1.,0.));
#14730=DIRECTION('ref_axis',(1.,0.,0.));
#14731=DIRECTION('',(0.,-1.,0.));
#14732=DIRECTION('center_axis',(0.,-1.,0.));
#14733=DIRECTION('ref_axis',(1.,0.,0.));
#14734=DIRECTION('center_axis',(0.,1.,0.));
#14735=DIRECTION('ref_axis',(1.,0.,0.));
#14736=DIRECTION('center_axis',(0.,-1.,0.));
#14737=DIRECTION('ref_axis',(1.,0.,0.));
#14738=DIRECTION('',(0.,-1.,0.));
#14739=DIRECTION('center_axis',(0.,-1.,0.));
#14740=DIRECTION('ref_axis',(1.,0.,0.));
#14741=DIRECTION('center_axis',(0.,1.,0.));
#14742=DIRECTION('ref_axis',(1.,0.,0.));
#14743=DIRECTION('center_axis',(0.,-1.,0.));
#14744=DIRECTION('ref_axis',(1.,0.,0.));
#14745=DIRECTION('',(0.,-1.,0.));
#14746=DIRECTION('center_axis',(0.,-1.,0.));
#14747=DIRECTION('ref_axis',(1.,0.,0.));
#14748=DIRECTION('center_axis',(0.,1.,0.));
#14749=DIRECTION('ref_axis',(1.,0.,0.));
#14750=DIRECTION('center_axis',(0.,-1.,0.));
#14751=DIRECTION('ref_axis',(1.,0.,0.));
#14752=DIRECTION('',(0.,-1.,0.));
#14753=DIRECTION('center_axis',(0.,-1.,0.));
#14754=DIRECTION('ref_axis',(1.,0.,0.));
#14755=DIRECTION('center_axis',(0.,1.,0.));
#14756=DIRECTION('ref_axis',(1.,0.,0.));
#14757=DIRECTION('center_axis',(0.,-1.,0.));
#14758=DIRECTION('ref_axis',(1.,0.,0.));
#14759=DIRECTION('',(0.,-1.,0.));
#14760=DIRECTION('center_axis',(0.,-1.,0.));
#14761=DIRECTION('ref_axis',(1.,0.,0.));
#14762=DIRECTION('center_axis',(0.,1.,0.));
#14763=DIRECTION('ref_axis',(1.,0.,0.));
#14764=DIRECTION('center_axis',(0.,-1.,0.));
#14765=DIRECTION('ref_axis',(1.,0.,0.));
#14766=DIRECTION('',(0.,-1.,0.));
#14767=DIRECTION('center_axis',(0.,-1.,0.));
#14768=DIRECTION('ref_axis',(1.,0.,0.));
#14769=DIRECTION('center_axis',(0.,1.,0.));
#14770=DIRECTION('ref_axis',(1.,0.,0.));
#14771=DIRECTION('center_axis',(0.,-1.,0.));
#14772=DIRECTION('ref_axis',(1.,0.,0.));
#14773=DIRECTION('',(0.,-1.,0.));
#14774=DIRECTION('center_axis',(0.,-1.,0.));
#14775=DIRECTION('ref_axis',(1.,0.,0.));
#14776=DIRECTION('center_axis',(0.,1.,0.));
#14777=DIRECTION('ref_axis',(1.,0.,0.));
#14778=DIRECTION('center_axis',(0.,-1.,0.));
#14779=DIRECTION('ref_axis',(1.,0.,0.));
#14780=DIRECTION('',(0.,-1.,0.));
#14781=DIRECTION('center_axis',(0.,-1.,0.));
#14782=DIRECTION('ref_axis',(1.,0.,0.));
#14783=DIRECTION('center_axis',(0.,1.,0.));
#14784=DIRECTION('ref_axis',(1.,0.,0.));
#14785=DIRECTION('center_axis',(0.,-1.,0.));
#14786=DIRECTION('ref_axis',(1.,0.,0.));
#14787=DIRECTION('',(0.,-1.,0.));
#14788=DIRECTION('center_axis',(0.,-1.,0.));
#14789=DIRECTION('ref_axis',(1.,0.,0.));
#14790=DIRECTION('center_axis',(0.,1.,0.));
#14791=DIRECTION('ref_axis',(1.,0.,0.));
#14792=DIRECTION('center_axis',(0.,-1.,0.));
#14793=DIRECTION('ref_axis',(1.,0.,0.));
#14794=DIRECTION('',(0.,-1.,0.));
#14795=DIRECTION('center_axis',(0.,-1.,0.));
#14796=DIRECTION('ref_axis',(1.,0.,0.));
#14797=DIRECTION('center_axis',(0.,1.,0.));
#14798=DIRECTION('ref_axis',(1.,0.,0.));
#14799=DIRECTION('center_axis',(0.,-1.,0.));
#14800=DIRECTION('ref_axis',(1.,0.,0.));
#14801=DIRECTION('',(0.,-1.,0.));
#14802=DIRECTION('center_axis',(0.,-1.,0.));
#14803=DIRECTION('ref_axis',(1.,0.,0.));
#14804=DIRECTION('center_axis',(0.,1.,0.));
#14805=DIRECTION('ref_axis',(1.,0.,0.));
#14806=DIRECTION('center_axis',(0.,-1.,0.));
#14807=DIRECTION('ref_axis',(1.,0.,0.));
#14808=DIRECTION('',(0.,-1.,0.));
#14809=DIRECTION('center_axis',(0.,-1.,0.));
#14810=DIRECTION('ref_axis',(1.,0.,0.));
#14811=DIRECTION('center_axis',(0.,1.,0.));
#14812=DIRECTION('ref_axis',(1.,0.,0.));
#14813=DIRECTION('center_axis',(0.,-1.,0.));
#14814=DIRECTION('ref_axis',(1.,0.,0.));
#14815=DIRECTION('',(0.,-1.,0.));
#14816=DIRECTION('center_axis',(0.,-1.,0.));
#14817=DIRECTION('ref_axis',(1.,0.,0.));
#14818=DIRECTION('center_axis',(0.,1.,0.));
#14819=DIRECTION('ref_axis',(1.,0.,0.));
#14820=DIRECTION('center_axis',(0.,-1.,0.));
#14821=DIRECTION('ref_axis',(1.,0.,0.));
#14822=DIRECTION('',(0.,-1.,0.));
#14823=DIRECTION('center_axis',(0.,-1.,0.));
#14824=DIRECTION('ref_axis',(1.,0.,0.));
#14825=DIRECTION('center_axis',(0.,1.,0.));
#14826=DIRECTION('ref_axis',(1.,0.,0.));
#14827=DIRECTION('center_axis',(0.,-1.,0.));
#14828=DIRECTION('ref_axis',(1.,0.,0.));
#14829=DIRECTION('',(0.,-1.,0.));
#14830=DIRECTION('center_axis',(0.,-1.,0.));
#14831=DIRECTION('ref_axis',(1.,0.,0.));
#14832=DIRECTION('center_axis',(0.,1.,0.));
#14833=DIRECTION('ref_axis',(1.,0.,0.));
#14834=DIRECTION('center_axis',(0.,-1.,0.));
#14835=DIRECTION('ref_axis',(1.,0.,0.));
#14836=DIRECTION('',(0.,-1.,0.));
#14837=DIRECTION('center_axis',(0.,-1.,0.));
#14838=DIRECTION('ref_axis',(1.,0.,0.));
#14839=DIRECTION('center_axis',(0.,1.,0.));
#14840=DIRECTION('ref_axis',(1.,0.,0.));
#14841=DIRECTION('center_axis',(0.,-1.,0.));
#14842=DIRECTION('ref_axis',(1.,0.,0.));
#14843=DIRECTION('',(0.,-1.,0.));
#14844=DIRECTION('center_axis',(0.,-1.,0.));
#14845=DIRECTION('ref_axis',(1.,0.,0.));
#14846=DIRECTION('center_axis',(0.,1.,0.));
#14847=DIRECTION('ref_axis',(1.,0.,0.));
#14848=DIRECTION('center_axis',(0.,-1.,0.));
#14849=DIRECTION('ref_axis',(1.,0.,0.));
#14850=DIRECTION('',(0.,-1.,0.));
#14851=DIRECTION('center_axis',(0.,-1.,0.));
#14852=DIRECTION('ref_axis',(1.,0.,0.));
#14853=DIRECTION('center_axis',(0.,1.,0.));
#14854=DIRECTION('ref_axis',(1.,0.,0.));
#14855=DIRECTION('center_axis',(0.,-1.,0.));
#14856=DIRECTION('ref_axis',(1.,0.,0.));
#14857=DIRECTION('',(0.,-1.,0.));
#14858=DIRECTION('center_axis',(0.,-1.,0.));
#14859=DIRECTION('ref_axis',(1.,0.,0.));
#14860=DIRECTION('center_axis',(0.,1.,0.));
#14861=DIRECTION('ref_axis',(1.,0.,0.));
#14862=DIRECTION('center_axis',(0.,-1.,0.));
#14863=DIRECTION('ref_axis',(1.,0.,0.));
#14864=DIRECTION('',(0.,-1.,0.));
#14865=DIRECTION('center_axis',(0.,-1.,0.));
#14866=DIRECTION('ref_axis',(1.,0.,0.));
#14867=DIRECTION('center_axis',(0.,1.,0.));
#14868=DIRECTION('ref_axis',(1.,0.,0.));
#14869=DIRECTION('center_axis',(0.,-1.,0.));
#14870=DIRECTION('ref_axis',(1.,0.,0.));
#14871=DIRECTION('',(0.,-1.,0.));
#14872=DIRECTION('center_axis',(0.,-1.,0.));
#14873=DIRECTION('ref_axis',(1.,0.,0.));
#14874=DIRECTION('center_axis',(0.,1.,0.));
#14875=DIRECTION('ref_axis',(1.,0.,0.));
#14876=DIRECTION('center_axis',(0.,-1.,0.));
#14877=DIRECTION('ref_axis',(1.,0.,0.));
#14878=DIRECTION('',(0.,-1.,0.));
#14879=DIRECTION('center_axis',(0.,-1.,0.));
#14880=DIRECTION('ref_axis',(1.,0.,0.));
#14881=DIRECTION('center_axis',(0.,1.,0.));
#14882=DIRECTION('ref_axis',(1.,0.,0.));
#14883=DIRECTION('center_axis',(0.,-1.,0.));
#14884=DIRECTION('ref_axis',(1.,0.,0.));
#14885=DIRECTION('',(0.,-1.,0.));
#14886=DIRECTION('center_axis',(0.,-1.,0.));
#14887=DIRECTION('ref_axis',(1.,0.,0.));
#14888=DIRECTION('center_axis',(0.,1.,0.));
#14889=DIRECTION('ref_axis',(1.,0.,0.));
#14890=DIRECTION('center_axis',(0.,-1.,0.));
#14891=DIRECTION('ref_axis',(1.,0.,0.));
#14892=DIRECTION('',(0.,-1.,0.));
#14893=DIRECTION('center_axis',(0.,-1.,0.));
#14894=DIRECTION('ref_axis',(1.,0.,0.));
#14895=DIRECTION('center_axis',(0.,1.,0.));
#14896=DIRECTION('ref_axis',(1.,0.,0.));
#14897=DIRECTION('center_axis',(0.,-1.,0.));
#14898=DIRECTION('ref_axis',(1.,0.,0.));
#14899=DIRECTION('',(0.,-1.,0.));
#14900=DIRECTION('center_axis',(0.,-1.,0.));
#14901=DIRECTION('ref_axis',(1.,0.,0.));
#14902=DIRECTION('center_axis',(0.,1.,0.));
#14903=DIRECTION('ref_axis',(1.,0.,0.));
#14904=DIRECTION('center_axis',(0.,-1.,0.));
#14905=DIRECTION('ref_axis',(1.,0.,0.));
#14906=DIRECTION('',(0.,-1.,0.));
#14907=DIRECTION('center_axis',(0.,-1.,0.));
#14908=DIRECTION('ref_axis',(1.,0.,0.));
#14909=DIRECTION('center_axis',(0.,1.,0.));
#14910=DIRECTION('ref_axis',(1.,0.,0.));
#14911=DIRECTION('center_axis',(0.,-1.,0.));
#14912=DIRECTION('ref_axis',(1.,0.,0.));
#14913=DIRECTION('',(0.,-1.,0.));
#14914=DIRECTION('center_axis',(0.,-1.,0.));
#14915=DIRECTION('ref_axis',(1.,0.,0.));
#14916=DIRECTION('center_axis',(0.,1.,0.));
#14917=DIRECTION('ref_axis',(1.,0.,0.));
#14918=DIRECTION('center_axis',(0.,-1.,0.));
#14919=DIRECTION('ref_axis',(1.,0.,0.));
#14920=DIRECTION('',(0.,-1.,0.));
#14921=DIRECTION('center_axis',(0.,-1.,0.));
#14922=DIRECTION('ref_axis',(1.,0.,0.));
#14923=DIRECTION('center_axis',(0.,1.,0.));
#14924=DIRECTION('ref_axis',(1.,0.,0.));
#14925=DIRECTION('center_axis',(0.,-1.,0.));
#14926=DIRECTION('ref_axis',(1.,0.,0.));
#14927=DIRECTION('',(0.,-1.,0.));
#14928=DIRECTION('center_axis',(0.,-1.,0.));
#14929=DIRECTION('ref_axis',(1.,0.,0.));
#14930=DIRECTION('center_axis',(0.,1.,0.));
#14931=DIRECTION('ref_axis',(1.,0.,0.));
#14932=DIRECTION('center_axis',(0.,-1.,0.));
#14933=DIRECTION('ref_axis',(1.,0.,0.));
#14934=DIRECTION('',(0.,-1.,0.));
#14935=DIRECTION('center_axis',(0.,-1.,0.));
#14936=DIRECTION('ref_axis',(1.,0.,0.));
#14937=DIRECTION('center_axis',(0.,1.,0.));
#14938=DIRECTION('ref_axis',(1.,0.,0.));
#14939=DIRECTION('center_axis',(0.,-1.,0.));
#14940=DIRECTION('ref_axis',(1.,0.,0.));
#14941=DIRECTION('',(0.,-1.,0.));
#14942=DIRECTION('center_axis',(0.,-1.,0.));
#14943=DIRECTION('ref_axis',(1.,0.,0.));
#14944=DIRECTION('center_axis',(0.,1.,0.));
#14945=DIRECTION('ref_axis',(1.,0.,0.));
#14946=DIRECTION('center_axis',(0.,-1.,0.));
#14947=DIRECTION('ref_axis',(1.,0.,0.));
#14948=DIRECTION('',(0.,-1.,0.));
#14949=DIRECTION('center_axis',(0.,-1.,0.));
#14950=DIRECTION('ref_axis',(1.,0.,0.));
#14951=DIRECTION('center_axis',(0.,1.,0.));
#14952=DIRECTION('ref_axis',(1.,0.,0.));
#14953=DIRECTION('center_axis',(0.,-1.,0.));
#14954=DIRECTION('ref_axis',(1.,0.,0.));
#14955=DIRECTION('',(0.,-1.,0.));
#14956=DIRECTION('center_axis',(0.,-1.,0.));
#14957=DIRECTION('ref_axis',(1.,0.,0.));
#14958=DIRECTION('center_axis',(0.,1.,0.));
#14959=DIRECTION('ref_axis',(1.,0.,0.));
#14960=DIRECTION('center_axis',(0.,-1.,0.));
#14961=DIRECTION('ref_axis',(1.,0.,0.));
#14962=DIRECTION('',(0.,-1.,0.));
#14963=DIRECTION('center_axis',(0.,-1.,0.));
#14964=DIRECTION('ref_axis',(1.,0.,0.));
#14965=DIRECTION('center_axis',(0.,1.,0.));
#14966=DIRECTION('ref_axis',(1.,0.,0.));
#14967=DIRECTION('center_axis',(0.,-1.,0.));
#14968=DIRECTION('ref_axis',(1.,0.,0.));
#14969=DIRECTION('',(0.,-1.,0.));
#14970=DIRECTION('center_axis',(0.,-1.,0.));
#14971=DIRECTION('ref_axis',(1.,0.,0.));
#14972=DIRECTION('center_axis',(0.,1.,0.));
#14973=DIRECTION('ref_axis',(1.,0.,0.));
#14974=DIRECTION('center_axis',(0.,-1.,0.));
#14975=DIRECTION('ref_axis',(1.,0.,0.));
#14976=DIRECTION('',(0.,-1.,0.));
#14977=DIRECTION('center_axis',(0.,-1.,0.));
#14978=DIRECTION('ref_axis',(1.,0.,0.));
#14979=DIRECTION('center_axis',(0.,1.,0.));
#14980=DIRECTION('ref_axis',(1.,0.,0.));
#14981=DIRECTION('center_axis',(0.,-1.,0.));
#14982=DIRECTION('ref_axis',(1.,0.,0.));
#14983=DIRECTION('',(0.,-1.,0.));
#14984=DIRECTION('center_axis',(0.,-1.,0.));
#14985=DIRECTION('ref_axis',(1.,0.,0.));
#14986=DIRECTION('center_axis',(0.,1.,0.));
#14987=DIRECTION('ref_axis',(1.,0.,0.));
#14988=DIRECTION('center_axis',(0.,-1.,0.));
#14989=DIRECTION('ref_axis',(1.,0.,0.));
#14990=DIRECTION('',(0.,-1.,0.));
#14991=DIRECTION('center_axis',(0.,-1.,0.));
#14992=DIRECTION('ref_axis',(1.,0.,0.));
#14993=DIRECTION('center_axis',(0.,1.,0.));
#14994=DIRECTION('ref_axis',(1.,0.,0.));
#14995=DIRECTION('center_axis',(0.,-1.,0.));
#14996=DIRECTION('ref_axis',(1.,0.,0.));
#14997=DIRECTION('',(0.,-1.,0.));
#14998=DIRECTION('center_axis',(0.,-1.,0.));
#14999=DIRECTION('ref_axis',(1.,0.,0.));
#15000=DIRECTION('center_axis',(0.,1.,0.));
#15001=DIRECTION('ref_axis',(1.,0.,0.));
#15002=DIRECTION('center_axis',(0.,-1.,0.));
#15003=DIRECTION('ref_axis',(1.,0.,0.));
#15004=DIRECTION('',(0.,-1.,0.));
#15005=DIRECTION('center_axis',(0.,-1.,0.));
#15006=DIRECTION('ref_axis',(1.,0.,0.));
#15007=DIRECTION('center_axis',(0.,0.,-1.));
#15008=DIRECTION('ref_axis',(-1.,0.,0.));
#15009=DIRECTION('',(1.,0.,0.));
#15010=DIRECTION('',(-1.,0.,0.));
#15011=DIRECTION('',(0.,1.,0.));
#15012=DIRECTION('center_axis',(1.,0.,0.));
#15013=DIRECTION('ref_axis',(0.,0.,-1.));
#15014=DIRECTION('',(0.,0.,1.));
#15015=DIRECTION('',(0.,0.,-1.));
#15016=DIRECTION('center_axis',(0.,1.,0.));
#15017=DIRECTION('ref_axis',(1.,0.,0.));
#15018=DIRECTION('center_axis',(0.,1.,0.));
#15019=DIRECTION('ref_axis',(1.,0.,0.));
#15020=DIRECTION('axis',(0.,0.,1.));
#15021=DIRECTION('refdir',(1.,0.,0.));
#15022=DIRECTION('center_axis',(0.,1.,0.));
#15023=DIRECTION('ref_axis',(1.,0.,0.));
#15024=DIRECTION('center_axis',(0.,1.,0.));
#15025=DIRECTION('ref_axis',(1.,0.,0.));
#15026=DIRECTION('',(0.,1.,0.));
#15027=DIRECTION('center_axis',(0.,-1.,0.));
#15028=DIRECTION('ref_axis',(1.,0.,0.));
#15029=DIRECTION('center_axis',(0.,-1.,0.));
#15030=DIRECTION('ref_axis',(-1.,0.,0.));
#15031=DIRECTION('center_axis',(0.,-1.,0.));
#15032=DIRECTION('ref_axis',(-1.,0.,0.));
#15033=DIRECTION('',(0.,-1.,0.));
#15034=DIRECTION('center_axis',(0.,1.,0.));
#15035=DIRECTION('ref_axis',(-1.,0.,0.));
#15036=DIRECTION('center_axis',(0.,-1.,0.));
#15037=DIRECTION('ref_axis',(-1.,0.,0.));
#15038=DIRECTION('center_axis',(0.,-1.,0.));
#15039=DIRECTION('ref_axis',(-1.,0.,0.));
#15040=DIRECTION('',(0.,-1.,0.));
#15041=DIRECTION('center_axis',(0.,1.,0.));
#15042=DIRECTION('ref_axis',(-1.,0.,0.));
#15043=DIRECTION('center_axis',(-1.,0.,0.));
#15044=DIRECTION('ref_axis',(0.,0.707106781186546,0.707106781186549));
#15045=DIRECTION('center_axis',(1.,0.,0.));
#15046=DIRECTION('ref_axis',(0.,0.707106781186546,0.707106781186549));
#15047=DIRECTION('',(-1.,0.,0.));
#15048=DIRECTION('center_axis',(-1.,0.,0.));
#15049=DIRECTION('ref_axis',(0.,0.707106781186546,0.707106781186549));
#15050=DIRECTION('',(1.,0.,0.));
#15051=DIRECTION('center_axis',(0.,0.,1.));
#15052=DIRECTION('ref_axis',(1.,0.,0.));
#15053=DIRECTION('',(0.,-1.,0.));
#15054=DIRECTION('',(-0.707106781186546,0.707106781186549,0.));
#15055=DIRECTION('',(-0.707106781186546,-0.707106781186549,0.));
#15056=DIRECTION('',(-1.,0.,0.));
#15057=DIRECTION('',(0.707106781186546,-0.707106781186549,0.));
#15058=DIRECTION('',(0.707106781186546,0.707106781186549,0.));
#15059=DIRECTION('',(0.,1.,0.));
#15060=DIRECTION('center_axis',(0.,0.,-1.));
#15061=DIRECTION('ref_axis',(1.,0.,0.));
#15062=DIRECTION('center_axis',(0.,0.,-1.));
#15063=DIRECTION('ref_axis',(1.,0.,0.));
#15064=DIRECTION('center_axis',(0.,0.,-1.));
#15065=DIRECTION('ref_axis',(1.,0.,0.));
#15066=DIRECTION('center_axis',(0.,0.,-1.));
#15067=DIRECTION('ref_axis',(1.,0.,0.));
#15068=DIRECTION('center_axis',(0.,0.,-1.));
#15069=DIRECTION('ref_axis',(1.,0.,0.));
#15070=DIRECTION('center_axis',(0.,0.,-1.));
#15071=DIRECTION('ref_axis',(1.,0.,0.));
#15072=DIRECTION('center_axis',(0.,0.,-1.));
#15073=DIRECTION('ref_axis',(1.,0.,0.));
#15074=DIRECTION('center_axis',(0.,0.,-1.));
#15075=DIRECTION('ref_axis',(1.,0.,0.));
#15076=DIRECTION('center_axis',(0.,0.,-1.));
#15077=DIRECTION('ref_axis',(1.,0.,0.));
#15078=DIRECTION('center_axis',(0.,0.,-1.));
#15079=DIRECTION('ref_axis',(1.,0.,0.));
#15080=DIRECTION('center_axis',(0.,0.,-1.));
#15081=DIRECTION('ref_axis',(1.,0.,0.));
#15082=DIRECTION('center_axis',(1.,0.,0.));
#15083=DIRECTION('ref_axis',(0.,0.992156741649222,0.125));
#15084=DIRECTION('center_axis',(1.,0.,0.));
#15085=DIRECTION('ref_axis',(0.,0.992156741649222,0.125));
#15086=DIRECTION('',(1.,0.,0.));
#15087=DIRECTION('center_axis',(-1.,0.,0.));
#15088=DIRECTION('ref_axis',(0.,0.992156741649222,0.125));
#15089=DIRECTION('',(1.,0.,0.));
#15090=DIRECTION('center_axis',(0.,0.,1.));
#15091=DIRECTION('ref_axis',(1.,0.,0.));
#15092=DIRECTION('',(0.,-1.,0.));
#15093=DIRECTION('',(-0.707106781186546,-0.707106781186549,0.));
#15094=DIRECTION('',(0.707106781186546,-0.707106781186549,0.));
#15095=DIRECTION('',(1.,0.,0.));
#15096=DIRECTION('',(0.707106781186546,0.707106781186549,0.));
#15097=DIRECTION('',(-0.707106781186546,0.707106781186549,0.));
#15098=DIRECTION('',(0.,1.,0.));
#15099=DIRECTION('center_axis',(0.,0.,-1.));
#15100=DIRECTION('ref_axis',(1.,0.,0.));
#15101=DIRECTION('center_axis',(0.,0.,-1.));
#15102=DIRECTION('ref_axis',(1.,0.,0.));
#15103=DIRECTION('center_axis',(0.,0.,-1.));
#15104=DIRECTION('ref_axis',(1.,0.,0.));
#15105=DIRECTION('center_axis',(0.,0.,-1.));
#15106=DIRECTION('ref_axis',(1.,0.,0.));
#15107=DIRECTION('center_axis',(0.,0.,-1.));
#15108=DIRECTION('ref_axis',(1.,0.,0.));
#15109=DIRECTION('center_axis',(0.,0.,-1.));
#15110=DIRECTION('ref_axis',(1.,0.,0.));
#15111=DIRECTION('center_axis',(0.,0.,-1.));
#15112=DIRECTION('ref_axis',(1.,0.,0.));
#15113=DIRECTION('center_axis',(0.,0.,-1.));
#15114=DIRECTION('ref_axis',(1.,0.,0.));
#15115=DIRECTION('center_axis',(0.,0.,-1.));
#15116=DIRECTION('ref_axis',(1.,0.,0.));
#15117=DIRECTION('center_axis',(0.,0.,-1.));
#15118=DIRECTION('ref_axis',(1.,0.,0.));
#15119=DIRECTION('center_axis',(0.,0.,-1.));
#15120=DIRECTION('ref_axis',(1.,0.,0.));
#15121=DIRECTION('center_axis',(0.,0.,1.));
#15122=DIRECTION('ref_axis',(1.,0.,0.));
#15123=DIRECTION('',(0.,0.,-1.));
#15124=DIRECTION('center_axis',(0.,0.,1.));
#15125=DIRECTION('ref_axis',(1.,0.,0.));
#15126=DIRECTION('',(0.,0.,-1.));
#15127=DIRECTION('center_axis',(0.,0.,1.));
#15128=DIRECTION('ref_axis',(1.,0.,0.));
#15129=DIRECTION('',(0.,0.,-1.));
#15130=DIRECTION('center_axis',(0.,0.,1.));
#15131=DIRECTION('ref_axis',(1.,0.,0.));
#15132=DIRECTION('',(0.,0.,-1.));
#15133=DIRECTION('center_axis',(0.,0.,1.));
#15134=DIRECTION('ref_axis',(1.,0.,0.));
#15135=DIRECTION('',(0.,0.,-1.));
#15136=DIRECTION('center_axis',(0.,0.,1.));
#15137=DIRECTION('ref_axis',(1.,0.,0.));
#15138=DIRECTION('',(0.,0.,-1.));
#15139=DIRECTION('center_axis',(0.,0.,1.));
#15140=DIRECTION('ref_axis',(1.,0.,0.));
#15141=DIRECTION('',(0.,0.,-1.));
#15142=DIRECTION('center_axis',(0.,0.,1.));
#15143=DIRECTION('ref_axis',(1.,0.,0.));
#15144=DIRECTION('',(0.,0.,-1.));
#15145=DIRECTION('center_axis',(0.,0.,1.));
#15146=DIRECTION('ref_axis',(1.,0.,0.));
#15147=DIRECTION('',(0.,0.,-1.));
#15148=DIRECTION('center_axis',(0.,0.,1.));
#15149=DIRECTION('ref_axis',(1.,0.,0.));
#15150=DIRECTION('',(0.,0.,-1.));
#15151=DIRECTION('center_axis',(0.,0.,1.));
#15152=DIRECTION('ref_axis',(1.,0.,0.));
#15153=DIRECTION('',(0.,0.,-1.));
#15154=DIRECTION('center_axis',(-0.707106781186549,0.707106781186546,0.));
#15155=DIRECTION('ref_axis',(-0.707106781186546,-0.707106781186549,0.));
#15156=DIRECTION('',(0.,0.,1.));
#15157=DIRECTION('',(0.,0.,1.));
#15158=DIRECTION('center_axis',(0.707106781186549,0.707106781186546,0.));
#15159=DIRECTION('ref_axis',(-0.707106781186546,0.707106781186549,0.));
#15160=DIRECTION('',(0.,0.,1.));
#15161=DIRECTION('',(0.,0.,1.));
#15162=DIRECTION('center_axis',(0.707106781186549,-0.707106781186546,0.));
#15163=DIRECTION('ref_axis',(0.707106781186546,0.707106781186549,0.));
#15164=DIRECTION('',(0.,0.,1.));
#15165=DIRECTION('center_axis',(0.,-1.,0.));
#15166=DIRECTION('ref_axis',(1.,0.,0.));
#15167=DIRECTION('',(0.,0.,1.));
#15168=DIRECTION('center_axis',(-0.707106781186549,-0.707106781186546,0.));
#15169=DIRECTION('ref_axis',(0.707106781186546,-0.707106781186549,0.));
#15170=DIRECTION('center_axis',(0.,0.,1.));
#15171=DIRECTION('ref_axis',(1.,0.,0.));
#15172=DIRECTION('',(-1.,0.,0.));
#15173=DIRECTION('',(0.,-1.,0.));
#15174=DIRECTION('',(-0.707106781186546,0.707106781186549,0.));
#15175=DIRECTION('',(-0.707106781186546,-0.707106781186549,0.));
#15176=DIRECTION('',(-1.,0.,0.));
#15177=DIRECTION('',(0.707106781186546,-0.707106781186549,0.));
#15178=DIRECTION('',(0.707106781186546,0.707106781186549,0.));
#15179=DIRECTION('',(0.,1.,0.));
#15180=DIRECTION('center_axis',(0.,0.,-1.));
#15181=DIRECTION('ref_axis',(1.,0.,0.));
#15182=DIRECTION('center_axis',(0.,0.,-1.));
#15183=DIRECTION('ref_axis',(1.,0.,0.));
#15184=DIRECTION('center_axis',(0.,0.,-1.));
#15185=DIRECTION('ref_axis',(1.,0.,0.));
#15186=DIRECTION('center_axis',(0.,0.,-1.));
#15187=DIRECTION('ref_axis',(1.,0.,0.));
#15188=DIRECTION('center_axis',(0.,0.,-1.));
#15189=DIRECTION('ref_axis',(1.,0.,0.));
#15190=DIRECTION('center_axis',(0.,0.,-1.));
#15191=DIRECTION('ref_axis',(1.,0.,0.));
#15192=DIRECTION('center_axis',(0.,0.,-1.));
#15193=DIRECTION('ref_axis',(1.,0.,0.));
#15194=DIRECTION('center_axis',(0.,0.,-1.));
#15195=DIRECTION('ref_axis',(1.,0.,0.));
#15196=DIRECTION('center_axis',(0.,0.,-1.));
#15197=DIRECTION('ref_axis',(1.,0.,0.));
#15198=DIRECTION('center_axis',(0.,0.,-1.));
#15199=DIRECTION('ref_axis',(1.,0.,0.));
#15200=DIRECTION('center_axis',(0.,0.,-1.));
#15201=DIRECTION('ref_axis',(1.,0.,0.));
#15202=DIRECTION('center_axis',(0.,0.,1.));
#15203=DIRECTION('ref_axis',(1.,0.,0.));
#15204=DIRECTION('center_axis',(0.,0.,-1.));
#15205=DIRECTION('ref_axis',(1.,0.,0.));
#15206=DIRECTION('',(0.,0.,-1.));
#15207=DIRECTION('center_axis',(0.,0.,1.));
#15208=DIRECTION('ref_axis',(1.,0.,0.));
#15209=DIRECTION('center_axis',(0.,0.,-1.));
#15210=DIRECTION('ref_axis',(1.,0.,0.));
#15211=DIRECTION('',(0.,0.,-1.));
#15212=DIRECTION('center_axis',(0.,0.,1.));
#15213=DIRECTION('ref_axis',(1.,0.,0.));
#15214=DIRECTION('center_axis',(0.,0.,-1.));
#15215=DIRECTION('ref_axis',(1.,0.,0.));
#15216=DIRECTION('',(0.,0.,-1.));
#15217=DIRECTION('center_axis',(0.,0.,1.));
#15218=DIRECTION('ref_axis',(1.,0.,0.));
#15219=DIRECTION('center_axis',(0.,0.,-1.));
#15220=DIRECTION('ref_axis',(1.,0.,0.));
#15221=DIRECTION('',(0.,0.,-1.));
#15222=DIRECTION('center_axis',(0.,0.,1.));
#15223=DIRECTION('ref_axis',(1.,0.,0.));
#15224=DIRECTION('center_axis',(0.,0.,-1.));
#15225=DIRECTION('ref_axis',(1.,0.,0.));
#15226=DIRECTION('',(0.,0.,-1.));
#15227=DIRECTION('center_axis',(0.,0.,1.));
#15228=DIRECTION('ref_axis',(1.,0.,0.));
#15229=DIRECTION('center_axis',(0.,0.,-1.));
#15230=DIRECTION('ref_axis',(1.,0.,0.));
#15231=DIRECTION('',(0.,0.,-1.));
#15232=DIRECTION('center_axis',(0.,0.,1.));
#15233=DIRECTION('ref_axis',(1.,0.,0.));
#15234=DIRECTION('center_axis',(0.,0.,-1.));
#15235=DIRECTION('ref_axis',(1.,0.,0.));
#15236=DIRECTION('',(0.,0.,-1.));
#15237=DIRECTION('center_axis',(0.,0.,1.));
#15238=DIRECTION('ref_axis',(1.,0.,0.));
#15239=DIRECTION('center_axis',(0.,0.,-1.));
#15240=DIRECTION('ref_axis',(1.,0.,0.));
#15241=DIRECTION('',(0.,0.,-1.));
#15242=DIRECTION('center_axis',(0.,0.,1.));
#15243=DIRECTION('ref_axis',(1.,0.,0.));
#15244=DIRECTION('center_axis',(0.,0.,-1.));
#15245=DIRECTION('ref_axis',(1.,0.,0.));
#15246=DIRECTION('',(0.,0.,-1.));
#15247=DIRECTION('center_axis',(0.,0.,1.));
#15248=DIRECTION('ref_axis',(1.,0.,0.));
#15249=DIRECTION('center_axis',(0.,0.,-1.));
#15250=DIRECTION('ref_axis',(1.,0.,0.));
#15251=DIRECTION('',(0.,0.,-1.));
#15252=DIRECTION('center_axis',(0.,0.,1.));
#15253=DIRECTION('ref_axis',(1.,0.,0.));
#15254=DIRECTION('center_axis',(0.,0.,-1.));
#15255=DIRECTION('ref_axis',(1.,0.,0.));
#15256=DIRECTION('',(0.,0.,-1.));
#15257=DIRECTION('center_axis',(-0.707106781186549,0.707106781186546,0.));
#15258=DIRECTION('ref_axis',(-0.707106781186546,-0.707106781186549,0.));
#15259=DIRECTION('',(0.,0.,1.));
#15260=DIRECTION('',(-0.707106781186546,-0.707106781186549,0.));
#15261=DIRECTION('',(0.,0.,1.));
#15262=DIRECTION('center_axis',(0.707106781186549,0.707106781186546,0.));
#15263=DIRECTION('ref_axis',(-0.707106781186546,0.707106781186549,0.));
#15264=DIRECTION('',(0.,0.,1.));
#15265=DIRECTION('',(-0.707106781186546,0.707106781186549,0.));
#15266=DIRECTION('',(0.,0.,1.));
#15267=DIRECTION('center_axis',(0.707106781186549,-0.707106781186546,0.));
#15268=DIRECTION('ref_axis',(0.707106781186546,0.707106781186549,0.));
#15269=DIRECTION('',(0.707106781186546,0.707106781186549,0.));
#15270=DIRECTION('',(0.,0.,1.));
#15271=DIRECTION('center_axis',(0.,-1.,0.));
#15272=DIRECTION('ref_axis',(1.,0.,0.));
#15273=DIRECTION('',(1.,0.,0.));
#15274=DIRECTION('',(0.,0.,1.));
#15275=DIRECTION('center_axis',(-0.707106781186549,-0.707106781186546,0.));
#15276=DIRECTION('ref_axis',(0.707106781186546,-0.707106781186549,0.));
#15277=DIRECTION('',(0.707106781186546,-0.707106781186549,0.));
#15278=DIRECTION('center_axis',(0.,0.,1.));
#15279=DIRECTION('ref_axis',(1.,0.,0.));
#15280=DIRECTION('',(1.,0.,0.));
#15281=DIRECTION('',(0.,-1.,0.));
#15282=DIRECTION('',(0.,1.,0.));
#15283=DIRECTION('center_axis',(0.,1.,0.));
#15284=DIRECTION('ref_axis',(1.,0.,0.));
#15285=DIRECTION('',(0.,0.,-1.));
#15286=DIRECTION('',(0.,0.,-1.));
#15287=DIRECTION('',(1.,0.,0.));
#15288=DIRECTION('center_axis',(0.,-1.,0.));
#15289=DIRECTION('ref_axis',(-1.,0.,0.));
#15290=DIRECTION('',(0.,0.,-1.));
#15291=DIRECTION('',(0.,0.,-1.));
#15292=DIRECTION('center_axis',(-1.,0.,0.));
#15293=DIRECTION('ref_axis',(0.,1.,0.));
#15294=DIRECTION('',(0.,1.,0.));
#15295=DIRECTION('',(0.,0.,-1.));
#15296=DIRECTION('center_axis',(0.,-1.,0.));
#15297=DIRECTION('ref_axis',(-1.,0.,0.));
#15298=DIRECTION('',(-1.,0.,0.));
#15299=DIRECTION('',(0.,0.,-1.));
#15300=DIRECTION('center_axis',(1.,0.,0.));
#15301=DIRECTION('ref_axis',(0.,-1.,0.));
#15302=DIRECTION('',(0.,-1.,0.));
#15303=DIRECTION('center_axis',(0.,0.,-1.));
#15304=DIRECTION('ref_axis',(-1.,0.,0.));
#15305=DIRECTION('axis',(0.,0.,1.));
#15306=DIRECTION('refdir',(1.,0.,0.));
#15307=DIRECTION('center_axis',(0.,-1.,0.));
#15308=DIRECTION('ref_axis',(-1.,0.,0.));
#15309=DIRECTION('center_axis',(0.,1.,0.));
#15310=DIRECTION('ref_axis',(-1.,0.,0.));
#15311=DIRECTION('',(0.,1.,0.));
#15312=DIRECTION('center_axis',(0.,1.,0.));
#15313=DIRECTION('ref_axis',(-1.,0.,0.));
#15314=DIRECTION('center_axis',(-0.866025403784439,0.,-0.499999999999999));
#15315=DIRECTION('ref_axis',(0.499999999999999,0.,-0.866025403784439));
#15316=DIRECTION('',(-0.499999999999999,0.,0.866025403784439));
#15317=DIRECTION('',(0.,-1.,0.));
#15318=DIRECTION('',(0.499999999999999,0.,-0.866025403784439));
#15319=DIRECTION('',(0.,-1.,0.));
#15320=DIRECTION('center_axis',(-0.866025403784439,0.,0.499999999999999));
#15321=DIRECTION('ref_axis',(-0.499999999999999,0.,-0.866025403784439));
#15322=DIRECTION('',(0.499999999999999,0.,0.866025403784439));
#15323=DIRECTION('',(-0.499999999999999,0.,-0.866025403784439));
#15324=DIRECTION('',(0.,-1.,0.));
#15325=DIRECTION('center_axis',(0.,0.,1.));
#15326=DIRECTION('ref_axis',(-1.,0.,0.));
#15327=DIRECTION('',(1.,0.,0.));
#15328=DIRECTION('',(-1.,0.,0.));
#15329=DIRECTION('',(0.,-1.,0.));
#15330=DIRECTION('center_axis',(0.866025403784438,0.,0.500000000000001));
#15331=DIRECTION('ref_axis',(-0.500000000000001,0.,0.866025403784438));
#15332=DIRECTION('',(0.500000000000001,0.,-0.866025403784438));
#15333=DIRECTION('',(-0.500000000000001,0.,0.866025403784438));
#15334=DIRECTION('',(0.,-1.,0.));
#15335=DIRECTION('center_axis',(0.866025403784439,0.,-0.5));
#15336=DIRECTION('ref_axis',(0.5,0.,0.866025403784439));
#15337=DIRECTION('',(-0.5,0.,-0.866025403784439));
#15338=DIRECTION('',(0.5,0.,0.866025403784439));
#15339=DIRECTION('',(0.,-1.,0.));
#15340=DIRECTION('center_axis',(4.61511044732058E-15,0.,-1.));
#15341=DIRECTION('ref_axis',(1.,0.,4.61511044732058E-15));
#15342=DIRECTION('',(-1.,0.,-4.61511044732058E-15));
#15343=DIRECTION('',(1.,0.,4.61511044732058E-15));
#15344=DIRECTION('center_axis',(0.,1.,0.));
#15345=DIRECTION('ref_axis',(-1.,0.,0.));
#15346=DIRECTION('center_axis',(0.,1.,0.));
#15347=DIRECTION('ref_axis',(-1.,0.,0.));
#15348=DIRECTION('axis',(0.,0.,1.));
#15349=DIRECTION('refdir',(1.,0.,0.));
#15350=DIRECTION('center_axis',(0.,1.,0.));
#15351=DIRECTION('ref_axis',(1.,0.,0.));
#15352=DIRECTION('center_axis',(0.,1.,0.));
#15353=DIRECTION('ref_axis',(1.,0.,0.));
#15354=DIRECTION('',(0.,1.,0.));
#15355=DIRECTION('center_axis',(0.,-1.,0.));
#15356=DIRECTION('ref_axis',(1.,0.,0.));
#15357=DIRECTION('center_axis',(0.,-1.,0.));
#15358=DIRECTION('ref_axis',(-1.,0.,0.));
#15359=DIRECTION('center_axis',(0.,-1.,0.));
#15360=DIRECTION('ref_axis',(-1.,0.,0.));
#15361=DIRECTION('',(0.,-1.,0.));
#15362=DIRECTION('center_axis',(0.,1.,0.));
#15363=DIRECTION('ref_axis',(-1.,0.,0.));
#15364=DIRECTION('center_axis',(0.,-1.,0.));
#15365=DIRECTION('ref_axis',(-1.,0.,0.));
#15366=DIRECTION('center_axis',(0.,-1.,0.));
#15367=DIRECTION('ref_axis',(-1.,0.,0.));
#15368=DIRECTION('',(0.,-1.,0.));
#15369=DIRECTION('center_axis',(0.,1.,0.));
#15370=DIRECTION('ref_axis',(-1.,0.,0.));
#15371=DIRECTION('center_axis',(-1.,0.,0.));
#15372=DIRECTION('ref_axis',(0.,0.707106781186546,0.707106781186549));
#15373=DIRECTION('center_axis',(1.,0.,0.));
#15374=DIRECTION('ref_axis',(0.,0.707106781186546,0.707106781186549));
#15375=DIRECTION('',(-1.,0.,0.));
#15376=DIRECTION('center_axis',(-1.,0.,0.));
#15377=DIRECTION('ref_axis',(0.,0.707106781186546,0.707106781186549));
#15378=DIRECTION('',(1.,0.,0.));
#15379=DIRECTION('center_axis',(0.,0.,1.));
#15380=DIRECTION('ref_axis',(1.,0.,0.));
#15381=DIRECTION('',(0.,-1.,0.));
#15382=DIRECTION('',(-0.707106781186546,0.707106781186549,0.));
#15383=DIRECTION('',(-0.707106781186546,-0.707106781186549,0.));
#15384=DIRECTION('',(-1.,0.,0.));
#15385=DIRECTION('',(0.707106781186546,-0.707106781186549,0.));
#15386=DIRECTION('',(0.707106781186546,0.707106781186549,0.));
#15387=DIRECTION('',(0.,1.,0.));
#15388=DIRECTION('center_axis',(0.,0.,-1.));
#15389=DIRECTION('ref_axis',(1.,0.,0.));
#15390=DIRECTION('center_axis',(0.,0.,-1.));
#15391=DIRECTION('ref_axis',(1.,0.,0.));
#15392=DIRECTION('center_axis',(0.,0.,-1.));
#15393=DIRECTION('ref_axis',(1.,0.,0.));
#15394=DIRECTION('center_axis',(0.,0.,-1.));
#15395=DIRECTION('ref_axis',(1.,0.,0.));
#15396=DIRECTION('center_axis',(0.,0.,-1.));
#15397=DIRECTION('ref_axis',(1.,0.,0.));
#15398=DIRECTION('center_axis',(0.,0.,-1.));
#15399=DIRECTION('ref_axis',(1.,0.,0.));
#15400=DIRECTION('center_axis',(0.,0.,-1.));
#15401=DIRECTION('ref_axis',(1.,0.,0.));
#15402=DIRECTION('center_axis',(0.,0.,-1.));
#15403=DIRECTION('ref_axis',(1.,0.,0.));
#15404=DIRECTION('center_axis',(0.,0.,-1.));
#15405=DIRECTION('ref_axis',(1.,0.,0.));
#15406=DIRECTION('center_axis',(0.,0.,-1.));
#15407=DIRECTION('ref_axis',(1.,0.,0.));
#15408=DIRECTION('center_axis',(0.,0.,-1.));
#15409=DIRECTION('ref_axis',(1.,0.,0.));
#15410=DIRECTION('center_axis',(1.,0.,0.));
#15411=DIRECTION('ref_axis',(0.,0.992156741649222,0.125));
#15412=DIRECTION('center_axis',(1.,0.,0.));
#15413=DIRECTION('ref_axis',(0.,0.992156741649222,0.125));
#15414=DIRECTION('',(1.,0.,0.));
#15415=DIRECTION('center_axis',(-1.,0.,0.));
#15416=DIRECTION('ref_axis',(0.,0.992156741649222,0.125));
#15417=DIRECTION('',(1.,0.,0.));
#15418=DIRECTION('center_axis',(0.,0.,1.));
#15419=DIRECTION('ref_axis',(1.,0.,0.));
#15420=DIRECTION('',(0.,-1.,0.));
#15421=DIRECTION('',(-0.707106781186546,-0.707106781186549,0.));
#15422=DIRECTION('',(0.707106781186546,-0.707106781186549,0.));
#15423=DIRECTION('',(1.,0.,0.));
#15424=DIRECTION('',(0.707106781186546,0.707106781186549,0.));
#15425=DIRECTION('',(-0.707106781186546,0.707106781186549,0.));
#15426=DIRECTION('',(0.,1.,0.));
#15427=DIRECTION('center_axis',(0.,0.,-1.));
#15428=DIRECTION('ref_axis',(1.,0.,0.));
#15429=DIRECTION('center_axis',(0.,0.,-1.));
#15430=DIRECTION('ref_axis',(1.,0.,0.));
#15431=DIRECTION('center_axis',(0.,0.,-1.));
#15432=DIRECTION('ref_axis',(1.,0.,0.));
#15433=DIRECTION('center_axis',(0.,0.,-1.));
#15434=DIRECTION('ref_axis',(1.,0.,0.));
#15435=DIRECTION('center_axis',(0.,0.,-1.));
#15436=DIRECTION('ref_axis',(1.,0.,0.));
#15437=DIRECTION('center_axis',(0.,0.,-1.));
#15438=DIRECTION('ref_axis',(1.,0.,0.));
#15439=DIRECTION('center_axis',(0.,0.,-1.));
#15440=DIRECTION('ref_axis',(1.,0.,0.));
#15441=DIRECTION('center_axis',(0.,0.,-1.));
#15442=DIRECTION('ref_axis',(1.,0.,0.));
#15443=DIRECTION('center_axis',(0.,0.,-1.));
#15444=DIRECTION('ref_axis',(1.,0.,0.));
#15445=DIRECTION('center_axis',(0.,0.,-1.));
#15446=DIRECTION('ref_axis',(1.,0.,0.));
#15447=DIRECTION('center_axis',(0.,0.,-1.));
#15448=DIRECTION('ref_axis',(1.,0.,0.));
#15449=DIRECTION('center_axis',(0.,0.,1.));
#15450=DIRECTION('ref_axis',(1.,0.,0.));
#15451=DIRECTION('',(0.,0.,-1.));
#15452=DIRECTION('center_axis',(0.,0.,1.));
#15453=DIRECTION('ref_axis',(1.,0.,0.));
#15454=DIRECTION('',(0.,0.,-1.));
#15455=DIRECTION('center_axis',(0.,0.,1.));
#15456=DIRECTION('ref_axis',(1.,0.,0.));
#15457=DIRECTION('',(0.,0.,-1.));
#15458=DIRECTION('center_axis',(0.,0.,1.));
#15459=DIRECTION('ref_axis',(1.,0.,0.));
#15460=DIRECTION('',(0.,0.,-1.));
#15461=DIRECTION('center_axis',(0.,0.,1.));
#15462=DIRECTION('ref_axis',(1.,0.,0.));
#15463=DIRECTION('',(0.,0.,-1.));
#15464=DIRECTION('center_axis',(0.,0.,1.));
#15465=DIRECTION('ref_axis',(1.,0.,0.));
#15466=DIRECTION('',(0.,0.,-1.));
#15467=DIRECTION('center_axis',(0.,0.,1.));
#15468=DIRECTION('ref_axis',(1.,0.,0.));
#15469=DIRECTION('',(0.,0.,-1.));
#15470=DIRECTION('center_axis',(0.,0.,1.));
#15471=DIRECTION('ref_axis',(1.,0.,0.));
#15472=DIRECTION('',(0.,0.,-1.));
#15473=DIRECTION('center_axis',(0.,0.,1.));
#15474=DIRECTION('ref_axis',(1.,0.,0.));
#15475=DIRECTION('',(0.,0.,-1.));
#15476=DIRECTION('center_axis',(0.,0.,1.));
#15477=DIRECTION('ref_axis',(1.,0.,0.));
#15478=DIRECTION('',(0.,0.,-1.));
#15479=DIRECTION('center_axis',(0.,0.,1.));
#15480=DIRECTION('ref_axis',(1.,0.,0.));
#15481=DIRECTION('',(0.,0.,-1.));
#15482=DIRECTION('center_axis',(-0.707106781186549,0.707106781186546,0.));
#15483=DIRECTION('ref_axis',(-0.707106781186546,-0.707106781186549,0.));
#15484=DIRECTION('',(0.,0.,1.));
#15485=DIRECTION('',(0.,0.,1.));
#15486=DIRECTION('center_axis',(0.707106781186549,0.707106781186546,0.));
#15487=DIRECTION('ref_axis',(-0.707106781186546,0.707106781186549,0.));
#15488=DIRECTION('',(0.,0.,1.));
#15489=DIRECTION('',(0.,0.,1.));
#15490=DIRECTION('center_axis',(0.707106781186549,-0.707106781186546,0.));
#15491=DIRECTION('ref_axis',(0.707106781186546,0.707106781186549,0.));
#15492=DIRECTION('',(0.,0.,1.));
#15493=DIRECTION('center_axis',(0.,-1.,0.));
#15494=DIRECTION('ref_axis',(1.,0.,0.));
#15495=DIRECTION('',(0.,0.,1.));
#15496=DIRECTION('center_axis',(-0.707106781186549,-0.707106781186546,0.));
#15497=DIRECTION('ref_axis',(0.707106781186546,-0.707106781186549,0.));
#15498=DIRECTION('center_axis',(0.,0.,1.));
#15499=DIRECTION('ref_axis',(1.,0.,0.));
#15500=DIRECTION('',(-1.,0.,0.));
#15501=DIRECTION('',(0.,-1.,0.));
#15502=DIRECTION('',(-0.707106781186546,0.707106781186549,0.));
#15503=DIRECTION('',(-0.707106781186546,-0.707106781186549,0.));
#15504=DIRECTION('',(-1.,0.,0.));
#15505=DIRECTION('',(0.707106781186546,-0.707106781186549,0.));
#15506=DIRECTION('',(0.707106781186546,0.707106781186549,0.));
#15507=DIRECTION('',(0.,1.,0.));
#15508=DIRECTION('center_axis',(0.,0.,-1.));
#15509=DIRECTION('ref_axis',(1.,0.,0.));
#15510=DIRECTION('center_axis',(0.,0.,-1.));
#15511=DIRECTION('ref_axis',(1.,0.,0.));
#15512=DIRECTION('center_axis',(0.,0.,-1.));
#15513=DIRECTION('ref_axis',(1.,0.,0.));
#15514=DIRECTION('center_axis',(0.,0.,-1.));
#15515=DIRECTION('ref_axis',(1.,0.,0.));
#15516=DIRECTION('center_axis',(0.,0.,-1.));
#15517=DIRECTION('ref_axis',(1.,0.,0.));
#15518=DIRECTION('center_axis',(0.,0.,-1.));
#15519=DIRECTION('ref_axis',(1.,0.,0.));
#15520=DIRECTION('center_axis',(0.,0.,-1.));
#15521=DIRECTION('ref_axis',(1.,0.,0.));
#15522=DIRECTION('center_axis',(0.,0.,-1.));
#15523=DIRECTION('ref_axis',(1.,0.,0.));
#15524=DIRECTION('center_axis',(0.,0.,-1.));
#15525=DIRECTION('ref_axis',(1.,0.,0.));
#15526=DIRECTION('center_axis',(0.,0.,-1.));
#15527=DIRECTION('ref_axis',(1.,0.,0.));
#15528=DIRECTION('center_axis',(0.,0.,-1.));
#15529=DIRECTION('ref_axis',(1.,0.,0.));
#15530=DIRECTION('center_axis',(0.,0.,1.));
#15531=DIRECTION('ref_axis',(1.,0.,0.));
#15532=DIRECTION('center_axis',(0.,0.,-1.));
#15533=DIRECTION('ref_axis',(1.,0.,0.));
#15534=DIRECTION('',(0.,0.,-1.));
#15535=DIRECTION('center_axis',(0.,0.,1.));
#15536=DIRECTION('ref_axis',(1.,0.,0.));
#15537=DIRECTION('center_axis',(0.,0.,-1.));
#15538=DIRECTION('ref_axis',(1.,0.,0.));
#15539=DIRECTION('',(0.,0.,-1.));
#15540=DIRECTION('center_axis',(0.,0.,1.));
#15541=DIRECTION('ref_axis',(1.,0.,0.));
#15542=DIRECTION('center_axis',(0.,0.,-1.));
#15543=DIRECTION('ref_axis',(1.,0.,0.));
#15544=DIRECTION('',(0.,0.,-1.));
#15545=DIRECTION('center_axis',(0.,0.,1.));
#15546=DIRECTION('ref_axis',(1.,0.,0.));
#15547=DIRECTION('center_axis',(0.,0.,-1.));
#15548=DIRECTION('ref_axis',(1.,0.,0.));
#15549=DIRECTION('',(0.,0.,-1.));
#15550=DIRECTION('center_axis',(0.,0.,1.));
#15551=DIRECTION('ref_axis',(1.,0.,0.));
#15552=DIRECTION('center_axis',(0.,0.,-1.));
#15553=DIRECTION('ref_axis',(1.,0.,0.));
#15554=DIRECTION('',(0.,0.,-1.));
#15555=DIRECTION('center_axis',(0.,0.,1.));
#15556=DIRECTION('ref_axis',(1.,0.,0.));
#15557=DIRECTION('center_axis',(0.,0.,-1.));
#15558=DIRECTION('ref_axis',(1.,0.,0.));
#15559=DIRECTION('',(0.,0.,-1.));
#15560=DIRECTION('center_axis',(0.,0.,1.));
#15561=DIRECTION('ref_axis',(1.,0.,0.));
#15562=DIRECTION('center_axis',(0.,0.,-1.));
#15563=DIRECTION('ref_axis',(1.,0.,0.));
#15564=DIRECTION('',(0.,0.,-1.));
#15565=DIRECTION('center_axis',(0.,0.,1.));
#15566=DIRECTION('ref_axis',(1.,0.,0.));
#15567=DIRECTION('center_axis',(0.,0.,-1.));
#15568=DIRECTION('ref_axis',(1.,0.,0.));
#15569=DIRECTION('',(0.,0.,-1.));
#15570=DIRECTION('center_axis',(0.,0.,1.));
#15571=DIRECTION('ref_axis',(1.,0.,0.));
#15572=DIRECTION('center_axis',(0.,0.,-1.));
#15573=DIRECTION('ref_axis',(1.,0.,0.));
#15574=DIRECTION('',(0.,0.,-1.));
#15575=DIRECTION('center_axis',(0.,0.,1.));
#15576=DIRECTION('ref_axis',(1.,0.,0.));
#15577=DIRECTION('center_axis',(0.,0.,-1.));
#15578=DIRECTION('ref_axis',(1.,0.,0.));
#15579=DIRECTION('',(0.,0.,-1.));
#15580=DIRECTION('center_axis',(0.,0.,1.));
#15581=DIRECTION('ref_axis',(1.,0.,0.));
#15582=DIRECTION('center_axis',(0.,0.,-1.));
#15583=DIRECTION('ref_axis',(1.,0.,0.));
#15584=DIRECTION('',(0.,0.,-1.));
#15585=DIRECTION('center_axis',(-0.707106781186549,0.707106781186546,0.));
#15586=DIRECTION('ref_axis',(-0.707106781186546,-0.707106781186549,0.));
#15587=DIRECTION('',(0.,0.,1.));
#15588=DIRECTION('',(-0.707106781186546,-0.707106781186549,0.));
#15589=DIRECTION('',(0.,0.,1.));
#15590=DIRECTION('center_axis',(0.707106781186549,0.707106781186546,0.));
#15591=DIRECTION('ref_axis',(-0.707106781186546,0.707106781186549,0.));
#15592=DIRECTION('',(0.,0.,1.));
#15593=DIRECTION('',(-0.707106781186546,0.707106781186549,0.));
#15594=DIRECTION('',(0.,0.,1.));
#15595=DIRECTION('center_axis',(0.707106781186549,-0.707106781186546,0.));
#15596=DIRECTION('ref_axis',(0.707106781186546,0.707106781186549,0.));
#15597=DIRECTION('',(0.707106781186546,0.707106781186549,0.));
#15598=DIRECTION('',(0.,0.,1.));
#15599=DIRECTION('center_axis',(0.,-1.,0.));
#15600=DIRECTION('ref_axis',(1.,0.,0.));
#15601=DIRECTION('',(1.,0.,0.));
#15602=DIRECTION('',(0.,0.,1.));
#15603=DIRECTION('center_axis',(-0.707106781186549,-0.707106781186546,0.));
#15604=DIRECTION('ref_axis',(0.707106781186546,-0.707106781186549,0.));
#15605=DIRECTION('',(0.707106781186546,-0.707106781186549,0.));
#15606=DIRECTION('center_axis',(0.,0.,1.));
#15607=DIRECTION('ref_axis',(1.,0.,0.));
#15608=DIRECTION('',(1.,0.,0.));
#15609=DIRECTION('',(0.,-1.,0.));
#15610=DIRECTION('',(0.,1.,0.));
#15611=DIRECTION('center_axis',(0.,1.,0.));
#15612=DIRECTION('ref_axis',(1.,0.,0.));
#15613=DIRECTION('',(0.,0.,-1.));
#15614=DIRECTION('',(0.,0.,-1.));
#15615=DIRECTION('',(1.,0.,0.));
#15616=DIRECTION('center_axis',(0.,-1.,0.));
#15617=DIRECTION('ref_axis',(-1.,0.,0.));
#15618=DIRECTION('',(0.,0.,-1.));
#15619=DIRECTION('',(0.,0.,-1.));
#15620=DIRECTION('center_axis',(-1.,0.,0.));
#15621=DIRECTION('ref_axis',(0.,1.,0.));
#15622=DIRECTION('',(0.,1.,0.));
#15623=DIRECTION('',(0.,0.,-1.));
#15624=DIRECTION('center_axis',(0.,-1.,0.));
#15625=DIRECTION('ref_axis',(-1.,0.,0.));
#15626=DIRECTION('',(-1.,0.,0.));
#15627=DIRECTION('',(0.,0.,-1.));
#15628=DIRECTION('center_axis',(1.,0.,0.));
#15629=DIRECTION('ref_axis',(0.,-1.,0.));
#15630=DIRECTION('',(0.,-1.,0.));
#15631=DIRECTION('center_axis',(0.,0.,-1.));
#15632=DIRECTION('ref_axis',(-1.,0.,0.));
#15633=DIRECTION('axis',(0.,0.,1.));
#15634=DIRECTION('refdir',(1.,0.,0.));
#15635=DIRECTION('center_axis',(0.,-1.,0.));
#15636=DIRECTION('ref_axis',(1.,0.,0.));
#15637=DIRECTION('',(0.427641188232285,0.,0.903948568297599));
#15638=DIRECTION('',(0.996663017976436,0.,0.0816261514350802));
#15639=DIRECTION('',(0.569021829744153,0.,-0.82232241686252));
#15640=DIRECTION('',(-0.427641188232283,0.,-0.9039485682976));
#15641=DIRECTION('',(-0.996663017976436,0.,-0.0816261514350783));
#15642=DIRECTION('',(-0.569021829744152,0.,0.822322416862521));
#15643=DIRECTION('center_axis',(0.,1.,0.));
#15644=DIRECTION('ref_axis',(1.,0.,0.));
#15645=DIRECTION('center_axis',(0.0816261514350802,0.,-0.996663017976436));
#15646=DIRECTION('ref_axis',(0.996663017976436,0.,0.0816261514350802));
#15647=DIRECTION('',(0.,-1.,0.));
#15648=DIRECTION('',(0.996663017976436,0.,0.0816261514350802));
#15649=DIRECTION('',(0.,-1.,0.));
#15650=DIRECTION('center_axis',(-0.82232241686252,0.,-0.569021829744153));
#15651=DIRECTION('ref_axis',(0.569021829744153,0.,-0.82232241686252));
#15652=DIRECTION('',(0.569021829744153,0.,-0.82232241686252));
#15653=DIRECTION('',(0.,-1.,0.));
#15654=DIRECTION('center_axis',(-0.9039485682976,0.,0.427641188232283));
#15655=DIRECTION('ref_axis',(-0.427641188232283,0.,-0.9039485682976));
#15656=DIRECTION('',(-0.427641188232283,0.,-0.9039485682976));
#15657=DIRECTION('',(0.,-1.,0.));
#15658=DIRECTION('center_axis',(-0.0816261514350783,0.,0.996663017976436));
#15659=DIRECTION('ref_axis',(-0.996663017976436,0.,-0.0816261514350783));
#15660=DIRECTION('',(-0.996663017976436,0.,-0.0816261514350783));
#15661=DIRECTION('',(0.,-1.,0.));
#15662=DIRECTION('center_axis',(0.822322416862521,0.,0.569021829744152));
#15663=DIRECTION('ref_axis',(-0.569021829744152,0.,0.822322416862521));
#15664=DIRECTION('',(-0.569021829744152,0.,0.822322416862521));
#15665=DIRECTION('',(0.,-1.,0.));
#15666=DIRECTION('center_axis',(0.903948568297599,0.,-0.427641188232285));
#15667=DIRECTION('ref_axis',(0.427641188232285,0.,0.903948568297599));
#15668=DIRECTION('',(0.427641188232285,0.,0.903948568297599));
#15669=DIRECTION('center_axis',(0.,-1.,0.));
#15670=DIRECTION('ref_axis',(1.,0.,0.));
#15671=DIRECTION('center_axis',(0.,1.,0.));
#15672=DIRECTION('ref_axis',(1.,0.,0.));
#15673=DIRECTION('center_axis',(0.,1.,0.));
#15674=DIRECTION('ref_axis',(1.,0.,0.));
#15675=DIRECTION('',(0.,-1.,0.));
#15676=DIRECTION('center_axis',(0.,-1.,0.));
#15677=DIRECTION('ref_axis',(1.,0.,0.));
#15678=DIRECTION('axis',(0.,0.,1.));
#15679=DIRECTION('refdir',(1.,0.,0.));
#15680=DIRECTION('center_axis',(0.,-1.,0.));
#15681=DIRECTION('ref_axis',(-1.,0.,0.));
#15682=DIRECTION('center_axis',(0.,1.,0.));
#15683=DIRECTION('ref_axis',(-1.,0.,0.));
#15684=DIRECTION('',(0.,1.,0.));
#15685=DIRECTION('center_axis',(0.,1.,0.));
#15686=DIRECTION('ref_axis',(-1.,0.,0.));
#15687=DIRECTION('center_axis',(-0.866025403784439,0.,-0.499999999999999));
#15688=DIRECTION('ref_axis',(0.499999999999999,0.,-0.866025403784439));
#15689=DIRECTION('',(-0.499999999999999,0.,0.866025403784439));
#15690=DIRECTION('',(0.,-1.,0.));
#15691=DIRECTION('',(0.499999999999999,0.,-0.866025403784439));
#15692=DIRECTION('',(0.,-1.,0.));
#15693=DIRECTION('center_axis',(-0.866025403784439,0.,0.499999999999999));
#15694=DIRECTION('ref_axis',(-0.499999999999999,0.,-0.866025403784439));
#15695=DIRECTION('',(0.499999999999999,0.,0.866025403784439));
#15696=DIRECTION('',(-0.499999999999999,0.,-0.866025403784439));
#15697=DIRECTION('',(0.,-1.,0.));
#15698=DIRECTION('center_axis',(0.,0.,1.));
#15699=DIRECTION('ref_axis',(-1.,0.,0.));
#15700=DIRECTION('',(1.,0.,0.));
#15701=DIRECTION('',(-1.,0.,0.));
#15702=DIRECTION('',(0.,-1.,0.));
#15703=DIRECTION('center_axis',(0.866025403784438,0.,0.500000000000001));
#15704=DIRECTION('ref_axis',(-0.500000000000001,0.,0.866025403784438));
#15705=DIRECTION('',(0.500000000000001,0.,-0.866025403784438));
#15706=DIRECTION('',(-0.500000000000001,0.,0.866025403784438));
#15707=DIRECTION('',(0.,-1.,0.));
#15708=DIRECTION('center_axis',(0.866025403784439,0.,-0.5));
#15709=DIRECTION('ref_axis',(0.5,0.,0.866025403784439));
#15710=DIRECTION('',(-0.5,0.,-0.866025403784439));
#15711=DIRECTION('',(0.5,0.,0.866025403784439));
#15712=DIRECTION('',(0.,-1.,0.));
#15713=DIRECTION('center_axis',(4.61511044732058E-15,0.,-1.));
#15714=DIRECTION('ref_axis',(1.,0.,4.61511044732058E-15));
#15715=DIRECTION('',(-1.,0.,-4.61511044732058E-15));
#15716=DIRECTION('',(1.,0.,4.61511044732058E-15));
#15717=DIRECTION('center_axis',(0.,1.,0.));
#15718=DIRECTION('ref_axis',(-1.,0.,0.));
#15719=DIRECTION('center_axis',(0.,1.,0.));
#15720=DIRECTION('ref_axis',(-1.,0.,0.));
#15721=DIRECTION('axis',(0.,0.,1.));
#15722=DIRECTION('refdir',(1.,0.,0.));
#15723=DIRECTION('center_axis',(0.,-1.,0.));
#15724=DIRECTION('ref_axis',(-1.,0.,0.));
#15725=DIRECTION('center_axis',(0.,1.,0.));
#15726=DIRECTION('ref_axis',(-1.,0.,0.));
#15727=DIRECTION('',(0.,1.,0.));
#15728=DIRECTION('center_axis',(0.,1.,0.));
#15729=DIRECTION('ref_axis',(-1.,0.,0.));
#15730=DIRECTION('center_axis',(-0.866025403784439,0.,-0.499999999999999));
#15731=DIRECTION('ref_axis',(0.499999999999999,0.,-0.866025403784439));
#15732=DIRECTION('',(-0.499999999999999,0.,0.866025403784439));
#15733=DIRECTION('',(0.,-1.,0.));
#15734=DIRECTION('',(0.499999999999999,0.,-0.866025403784439));
#15735=DIRECTION('',(0.,-1.,0.));
#15736=DIRECTION('center_axis',(-0.866025403784439,0.,0.499999999999999));
#15737=DIRECTION('ref_axis',(-0.499999999999999,0.,-0.866025403784439));
#15738=DIRECTION('',(0.499999999999999,0.,0.866025403784439));
#15739=DIRECTION('',(-0.499999999999999,0.,-0.866025403784439));
#15740=DIRECTION('',(0.,-1.,0.));
#15741=DIRECTION('center_axis',(0.,0.,1.));
#15742=DIRECTION('ref_axis',(-1.,0.,0.));
#15743=DIRECTION('',(1.,0.,0.));
#15744=DIRECTION('',(-1.,0.,0.));
#15745=DIRECTION('',(0.,-1.,0.));
#15746=DIRECTION('center_axis',(0.866025403784438,0.,0.500000000000001));
#15747=DIRECTION('ref_axis',(-0.500000000000001,0.,0.866025403784438));
#15748=DIRECTION('',(0.500000000000001,0.,-0.866025403784438));
#15749=DIRECTION('',(-0.500000000000001,0.,0.866025403784438));
#15750=DIRECTION('',(0.,-1.,0.));
#15751=DIRECTION('center_axis',(0.866025403784439,0.,-0.5));
#15752=DIRECTION('ref_axis',(0.5,0.,0.866025403784439));
#15753=DIRECTION('',(-0.5,0.,-0.866025403784439));
#15754=DIRECTION('',(0.5,0.,0.866025403784439));
#15755=DIRECTION('',(0.,-1.,0.));
#15756=DIRECTION('center_axis',(4.61511044732058E-15,0.,-1.));
#15757=DIRECTION('ref_axis',(1.,0.,4.61511044732058E-15));
#15758=DIRECTION('',(-1.,0.,-4.61511044732058E-15));
#15759=DIRECTION('',(1.,0.,4.61511044732058E-15));
#15760=DIRECTION('center_axis',(0.,1.,0.));
#15761=DIRECTION('ref_axis',(-1.,0.,0.));
#15762=DIRECTION('center_axis',(0.,1.,0.));
#15763=DIRECTION('ref_axis',(-1.,0.,0.));
#15764=DIRECTION('axis',(0.,0.,1.));
#15765=DIRECTION('refdir',(1.,0.,0.));
#15766=DIRECTION('center_axis',(0.,-0.984725314960397,0.174115059877505));
#15767=DIRECTION('ref_axis',(0.,0.174115059877505,0.984725314960397));
#15768=DIRECTION('',(0.,-0.174115059877505,-0.984725314960397));
#15769=DIRECTION('',(-1.,0.,0.));
#15770=DIRECTION('',(0.,0.174115059877505,0.984725314960397));
#15771=DIRECTION('',(-1.,0.,0.));
#15772=DIRECTION('center_axis',(1.,0.,0.));
#15773=DIRECTION('ref_axis',(0.,-0.821913269381079,-0.569612655771715));
#15774=DIRECTION('center_axis',(-1.,0.,0.));
#15775=DIRECTION('ref_axis',(0.,-0.821913269381079,-0.569612655771715));
#15776=DIRECTION('',(-1.,0.,0.));
#15777=DIRECTION('center_axis',(-1.,0.,0.));
#15778=DIRECTION('ref_axis',(0.,-0.821913269381079,-0.569612655771715));
#15779=DIRECTION('center_axis',(0.,-0.821913269381085,-0.569612655771705));
#15780=DIRECTION('ref_axis',(0.,-0.569612655771705,0.821913269381085));
#15781=DIRECTION('',(0.,0.569612655771705,-0.821913269381085));
#15782=DIRECTION('',(1.,0.,0.));
#15783=DIRECTION('',(0.,-0.569612655771705,0.821913269381085));
#15784=DIRECTION('center_axis',(0.,0.821913269381085,0.569612655771706));
#15785=DIRECTION('ref_axis',(0.,0.569612655771706,-0.821913269381085));
#15786=DIRECTION('',(0.,0.569612655771706,-0.821913269381085));
#15787=DIRECTION('',(-1.,0.,0.));
#15788=DIRECTION('',(0.,0.569612655771706,-0.821913269381085));
#15789=DIRECTION('',(-1.,0.,0.));
#15790=DIRECTION('center_axis',(1.,0.,0.));
#15791=DIRECTION('ref_axis',(0.,-0.821913269381079,-0.569612655771714));
#15792=DIRECTION('center_axis',(-1.,0.,0.));
#15793=DIRECTION('ref_axis',(0.,-0.821913269381079,-0.569612655771714));
#15794=DIRECTION('',(-1.,0.,0.));
#15795=DIRECTION('center_axis',(1.,0.,0.));
#15796=DIRECTION('ref_axis',(0.,-0.821913269381079,-0.569612655771714));
#15797=DIRECTION('center_axis',(0.,0.984725314960397,-0.174115059877505));
#15798=DIRECTION('ref_axis',(0.,-0.174115059877505,-0.984725314960397));
#15799=DIRECTION('',(0.,-0.174115059877505,-0.984725314960397));
#15800=DIRECTION('',(-1.,0.,0.));
#15801=DIRECTION('',(0.,-0.174115059877505,-0.984725314960397));
#15802=DIRECTION('center_axis',(1.,0.,0.));
#15803=DIRECTION('ref_axis',(0.,8.88178419700113E-15,1.));
#15804=DIRECTION('center_axis',(-1.,0.,0.));
#15805=DIRECTION('ref_axis',(0.,8.88178419700113E-15,1.));
#15806=DIRECTION('',(-1.,0.,0.));
#15807=DIRECTION('center_axis',(-1.,0.,0.));
#15808=DIRECTION('ref_axis',(0.,8.88178419700113E-15,1.));
#15809=DIRECTION('center_axis',(1.,0.,0.));
#15810=DIRECTION('ref_axis',(0.,0.,1.));
#15811=DIRECTION('center_axis',(-1.,0.,0.));
#15812=DIRECTION('ref_axis',(0.,0.,1.));
#15813=DIRECTION('center_axis',(1.,0.,0.));
#15814=DIRECTION('ref_axis',(0.,0.,1.));
#15815=DIRECTION('',(-1.,0.,0.));
#15816=DIRECTION('center_axis',(0.,-6.91402766832813E-16,-1.));
#15817=DIRECTION('ref_axis',(0.,-1.,6.91402766832813E-16));
#15818=DIRECTION('',(0.,-1.,6.91402766832813E-16));
#15819=DIRECTION('',(-1.,0.,0.));
#15820=DIRECTION('',(0.,1.,6.91402766832813E-16));
#15821=DIRECTION('center_axis',(0.,-0.984725314960397,-0.174115059877505));
#15822=DIRECTION('ref_axis',(0.,-0.174115059877505,0.984725314960397));
#15823=DIRECTION('',(0.,0.174115059877505,-0.984725314960397));
#15824=DIRECTION('',(-1.,0.,0.));
#15825=DIRECTION('',(0.,-0.174115059877505,0.984725314960397));
#15826=DIRECTION('',(-1.,0.,0.));
#15827=DIRECTION('center_axis',(-1.,0.,0.));
#15828=DIRECTION('ref_axis',(0.,0.821913269381079,-0.569612655771715));
#15829=DIRECTION('center_axis',(1.,0.,0.));
#15830=DIRECTION('ref_axis',(0.,0.821913269381079,-0.569612655771715));
#15831=DIRECTION('center_axis',(1.,0.,0.));
#15832=DIRECTION('ref_axis',(0.,0.821913269381079,-0.569612655771715));
#15833=DIRECTION('',(-1.,0.,0.));
#15834=DIRECTION('center_axis',(0.,-0.821913269381085,0.569612655771705));
#15835=DIRECTION('ref_axis',(0.,0.569612655771705,0.821913269381085));
#15836=DIRECTION('',(0.,-0.569612655771705,-0.821913269381085));
#15837=DIRECTION('',(0.,0.569612655771705,0.821913269381085));
#15838=DIRECTION('',(-1.,0.,0.));
#15839=DIRECTION('center_axis',(0.,0.821913269381085,-0.569612655771706));
#15840=DIRECTION('ref_axis',(0.,-0.569612655771706,-0.821913269381085));
#15841=DIRECTION('',(0.,-0.569612655771706,-0.821913269381085));
#15842=DIRECTION('',(1.,0.,0.));
#15843=DIRECTION('',(0.,-0.569612655771706,-0.821913269381085));
#15844=DIRECTION('',(-1.,0.,0.));
#15845=DIRECTION('center_axis',(-1.,0.,0.));
#15846=DIRECTION('ref_axis',(0.,0.821913269381079,-0.569612655771714));
#15847=DIRECTION('center_axis',(1.,0.,0.));
#15848=DIRECTION('ref_axis',(0.,0.821913269381079,-0.569612655771714));
#15849=DIRECTION('center_axis',(-1.,0.,0.));
#15850=DIRECTION('ref_axis',(0.,0.821913269381079,-0.569612655771714));
#15851=DIRECTION('',(-1.,0.,0.));
#15852=DIRECTION('center_axis',(0.,0.984725314960397,0.174115059877505));
#15853=DIRECTION('ref_axis',(0.,0.174115059877505,-0.984725314960397));
#15854=DIRECTION('',(0.,0.174115059877505,-0.984725314960397));
#15855=DIRECTION('',(0.,0.174115059877505,-0.984725314960397));
#15856=DIRECTION('',(-1.,0.,0.));
#15857=DIRECTION('center_axis',(-1.,0.,0.));
#15858=DIRECTION('ref_axis',(0.,-8.88178419700113E-15,1.));
#15859=DIRECTION('center_axis',(1.,0.,0.));
#15860=DIRECTION('ref_axis',(0.,-8.88178419700113E-15,1.));
#15861=DIRECTION('center_axis',(1.,0.,0.));
#15862=DIRECTION('ref_axis',(0.,-8.88178419700113E-15,1.));
#15863=DIRECTION('center_axis',(0.,0.,1.));
#15864=DIRECTION('ref_axis',(0.,1.,0.));
#15865=DIRECTION('',(0.,1.,0.));
#15866=DIRECTION('',(-1.,0.,0.));
#15867=DIRECTION('',(0.,-1.,0.));
#15868=DIRECTION('center_axis',(-1.,0.,0.));
#15869=DIRECTION('ref_axis',(0.,0.,1.));
#15870=DIRECTION('center_axis',(1.,0.,0.));
#15871=DIRECTION('ref_axis',(0.,0.,1.));
#15872=DIRECTION('center_axis',(-1.,0.,0.));
#15873=DIRECTION('ref_axis',(0.,0.,1.));
#15874=DIRECTION('center_axis',(0.,0.,1.));
#15875=DIRECTION('ref_axis',(0.,1.,0.));
#15876=DIRECTION('',(0.,1.,0.));
#15877=DIRECTION('',(-1.,0.,0.));
#15878=DIRECTION('',(0.,1.,0.));
#15879=DIRECTION('center_axis',(0.,0.,1.));
#15880=DIRECTION('ref_axis',(0.,1.,0.));
#15881=DIRECTION('',(0.,1.,0.));
#15882=DIRECTION('',(-1.,0.,0.));
#15883=DIRECTION('',(0.,1.,0.));
#15884=DIRECTION('center_axis',(0.,0.,1.));
#15885=DIRECTION('ref_axis',(0.,1.,0.));
#15886=DIRECTION('',(0.,1.,0.));
#15887=DIRECTION('',(0.,1.,0.));
#15888=DIRECTION('center_axis',(1.,0.,0.));
#15889=DIRECTION('ref_axis',(0.,0.707106781186555,-0.70710678118654));
#15890=DIRECTION('center_axis',(-1.,0.,0.));
#15891=DIRECTION('ref_axis',(0.,0.707106781186555,-0.70710678118654));
#15892=DIRECTION('',(-1.,0.,0.));
#15893=DIRECTION('center_axis',(-1.,0.,0.));
#15894=DIRECTION('ref_axis',(0.,0.707106781186555,-0.70710678118654));
#15895=DIRECTION('center_axis',(0.,0.707106781186548,-0.707106781186548));
#15896=DIRECTION('ref_axis',(0.,-0.707106781186548,-0.707106781186548));
#15897=DIRECTION('',(0.,0.707106781186547,0.707106781186547));
#15898=DIRECTION('',(-1.,0.,0.));
#15899=DIRECTION('',(0.,-0.707106781186547,-0.707106781186547));
#15900=DIRECTION('center_axis',(1.,0.,0.));
#15901=DIRECTION('ref_axis',(0.,0.98480775301221,-0.17364817766692));
#15902=DIRECTION('center_axis',(-1.,0.,0.));
#15903=DIRECTION('ref_axis',(0.,0.98480775301221,-0.17364817766692));
#15904=DIRECTION('',(-1.,0.,0.));
#15905=DIRECTION('center_axis',(-1.,0.,0.));
#15906=DIRECTION('ref_axis',(0.,0.98480775301221,-0.17364817766692));
#15907=DIRECTION('center_axis',(0.,0.984807753012208,-0.173648177666932));
#15908=DIRECTION('ref_axis',(0.,-0.173648177666932,-0.984807753012208));
#15909=DIRECTION('',(0.,0.173648177666932,0.984807753012208));
#15910=DIRECTION('',(-1.,0.,0.));
#15911=DIRECTION('',(0.,-0.173648177666932,-0.984807753012208));
#15912=DIRECTION('center_axis',(0.,0.,-1.));
#15913=DIRECTION('ref_axis',(0.,-1.,0.));
#15914=DIRECTION('',(0.,-1.,0.));
#15915=DIRECTION('',(-1.,0.,0.));
#15916=DIRECTION('',(0.,-1.,0.));
#15917=DIRECTION('center_axis',(0.,-0.984807753012208,0.173648177666932));
#15918=DIRECTION('ref_axis',(0.,0.173648177666932,0.984807753012208));
#15919=DIRECTION('',(0.,0.173648177666932,0.984807753012208));
#15920=DIRECTION('',(-1.,0.,0.));
#15921=DIRECTION('',(0.,0.173648177666932,0.984807753012208));
#15922=DIRECTION('center_axis',(1.,0.,0.));
#15923=DIRECTION('ref_axis',(0.,0.984807753012209,-0.173648177666926));
#15924=DIRECTION('center_axis',(-1.,0.,0.));
#15925=DIRECTION('ref_axis',(0.,0.984807753012209,-0.173648177666926));
#15926=DIRECTION('',(-1.,0.,0.));
#15927=DIRECTION('center_axis',(1.,0.,0.));
#15928=DIRECTION('ref_axis',(0.,0.984807753012209,-0.173648177666926));
#15929=DIRECTION('center_axis',(0.,-0.707106781186547,0.707106781186548));
#15930=DIRECTION('ref_axis',(0.,0.707106781186548,0.707106781186547));
#15931=DIRECTION('',(0.,0.707106781186548,0.707106781186547));
#15932=DIRECTION('',(-1.,0.,0.));
#15933=DIRECTION('',(0.,0.707106781186548,0.707106781186547));
#15934=DIRECTION('center_axis',(1.,0.,0.));
#15935=DIRECTION('ref_axis',(0.,0.707106781186551,-0.707106781186544));
#15936=DIRECTION('center_axis',(-1.,0.,0.));
#15937=DIRECTION('ref_axis',(0.,0.707106781186551,-0.707106781186544));
#15938=DIRECTION('',(-1.,0.,0.));
#15939=DIRECTION('center_axis',(1.,0.,0.));
#15940=DIRECTION('ref_axis',(0.,0.707106781186551,-0.707106781186544));
#15941=DIRECTION('center_axis',(0.,0.,-1.));
#15942=DIRECTION('ref_axis',(0.,-1.,0.));
#15943=DIRECTION('',(0.,-1.,0.));
#15944=DIRECTION('',(-1.,0.,0.));
#15945=DIRECTION('',(0.,1.,0.));
#15946=DIRECTION('center_axis',(-1.,0.,0.));
#15947=DIRECTION('ref_axis',(0.,-0.707106781186555,-0.70710678118654));
#15948=DIRECTION('center_axis',(1.,0.,0.));
#15949=DIRECTION('ref_axis',(0.,-0.707106781186555,-0.70710678118654));
#15950=DIRECTION('center_axis',(1.,0.,0.));
#15951=DIRECTION('ref_axis',(0.,-0.707106781186555,-0.70710678118654));
#15952=DIRECTION('',(-1.,0.,0.));
#15953=DIRECTION('center_axis',(0.,0.707106781186548,0.707106781186548));
#15954=DIRECTION('ref_axis',(0.,0.707106781186548,-0.707106781186548));
#15955=DIRECTION('',(0.,-0.707106781186547,0.707106781186547));
#15956=DIRECTION('',(0.,0.707106781186547,-0.707106781186547));
#15957=DIRECTION('',(-1.,0.,0.));
#15958=DIRECTION('center_axis',(-1.,0.,0.));
#15959=DIRECTION('ref_axis',(0.,-0.98480775301221,-0.17364817766692));
#15960=DIRECTION('center_axis',(1.,0.,0.));
#15961=DIRECTION('ref_axis',(0.,-0.98480775301221,-0.17364817766692));
#15962=DIRECTION('center_axis',(1.,0.,0.));
#15963=DIRECTION('ref_axis',(0.,-0.98480775301221,-0.17364817766692));
#15964=DIRECTION('',(-1.,0.,0.));
#15965=DIRECTION('center_axis',(0.,0.984807753012208,0.173648177666932));
#15966=DIRECTION('ref_axis',(0.,0.173648177666932,-0.984807753012208));
#15967=DIRECTION('',(0.,-0.173648177666932,0.984807753012208));
#15968=DIRECTION('',(0.,0.173648177666932,-0.984807753012208));
#15969=DIRECTION('',(-1.,0.,0.));
#15970=DIRECTION('center_axis',(0.,0.,1.));
#15971=DIRECTION('ref_axis',(0.,1.,0.));
#15972=DIRECTION('',(0.,1.,0.));
#15973=DIRECTION('',(0.,1.,0.));
#15974=DIRECTION('',(-1.,0.,0.));
#15975=DIRECTION('center_axis',(0.,-0.984807753012208,-0.173648177666932));
#15976=DIRECTION('ref_axis',(0.,-0.173648177666932,0.984807753012208));
#15977=DIRECTION('',(0.,-0.173648177666932,0.984807753012208));
#15978=DIRECTION('',(0.,-0.173648177666932,0.984807753012208));
#15979=DIRECTION('',(-1.,0.,0.));
#15980=DIRECTION('center_axis',(-1.,0.,0.));
#15981=DIRECTION('ref_axis',(0.,-0.984807753012209,-0.173648177666926));
#15982=DIRECTION('center_axis',(1.,0.,0.));
#15983=DIRECTION('ref_axis',(0.,-0.984807753012209,-0.173648177666926));
#15984=DIRECTION('center_axis',(-1.,0.,0.));
#15985=DIRECTION('ref_axis',(0.,-0.984807753012209,-0.173648177666926));
#15986=DIRECTION('',(-1.,0.,0.));
#15987=DIRECTION('center_axis',(0.,-0.707106781186547,-0.707106781186548));
#15988=DIRECTION('ref_axis',(0.,-0.707106781186548,0.707106781186547));
#15989=DIRECTION('',(0.,-0.707106781186548,0.707106781186547));
#15990=DIRECTION('',(0.,-0.707106781186548,0.707106781186547));
#15991=DIRECTION('',(-1.,0.,0.));
#15992=DIRECTION('center_axis',(-1.,0.,0.));
#15993=DIRECTION('ref_axis',(0.,-0.707106781186551,-0.707106781186544));
#15994=DIRECTION('center_axis',(1.,0.,0.));
#15995=DIRECTION('ref_axis',(0.,-0.707106781186551,-0.707106781186544));
#15996=DIRECTION('center_axis',(-1.,0.,0.));
#15997=DIRECTION('ref_axis',(0.,-0.707106781186551,-0.707106781186544));
#15998=DIRECTION('center_axis',(1.,0.,0.));
#15999=DIRECTION('ref_axis',(0.,1.,0.));
#16000=DIRECTION('center_axis',(1.,0.,0.));
#16001=DIRECTION('ref_axis',(0.,1.,0.));
#16002=DIRECTION('axis',(0.,0.,1.));
#16003=DIRECTION('refdir',(1.,0.,0.));
#16004=DIRECTION('center_axis',(0.,-1.,0.));
#16005=DIRECTION('ref_axis',(-1.,0.,0.));
#16006=DIRECTION('center_axis',(0.,1.,0.));
#16007=DIRECTION('ref_axis',(-1.,0.,0.));
#16008=DIRECTION('',(0.,1.,0.));
#16009=DIRECTION('center_axis',(0.,1.,0.));
#16010=DIRECTION('ref_axis',(-1.,0.,0.));
#16011=DIRECTION('center_axis',(-0.866025403784439,0.,-0.499999999999999));
#16012=DIRECTION('ref_axis',(0.499999999999999,0.,-0.866025403784439));
#16013=DIRECTION('',(-0.499999999999999,0.,0.866025403784439));
#16014=DIRECTION('',(0.,-1.,0.));
#16015=DIRECTION('',(0.499999999999999,0.,-0.866025403784439));
#16016=DIRECTION('',(0.,-1.,0.));
#16017=DIRECTION('center_axis',(-0.866025403784439,0.,0.499999999999999));
#16018=DIRECTION('ref_axis',(-0.499999999999999,0.,-0.866025403784439));
#16019=DIRECTION('',(0.499999999999999,0.,0.866025403784439));
#16020=DIRECTION('',(-0.499999999999999,0.,-0.866025403784439));
#16021=DIRECTION('',(0.,-1.,0.));
#16022=DIRECTION('center_axis',(0.,0.,1.));
#16023=DIRECTION('ref_axis',(-1.,0.,0.));
#16024=DIRECTION('',(1.,0.,0.));
#16025=DIRECTION('',(-1.,0.,0.));
#16026=DIRECTION('',(0.,-1.,0.));
#16027=DIRECTION('center_axis',(0.866025403784438,0.,0.500000000000001));
#16028=DIRECTION('ref_axis',(-0.500000000000001,0.,0.866025403784438));
#16029=DIRECTION('',(0.500000000000001,0.,-0.866025403784438));
#16030=DIRECTION('',(-0.500000000000001,0.,0.866025403784438));
#16031=DIRECTION('',(0.,-1.,0.));
#16032=DIRECTION('center_axis',(0.866025403784439,0.,-0.5));
#16033=DIRECTION('ref_axis',(0.5,0.,0.866025403784439));
#16034=DIRECTION('',(-0.5,0.,-0.866025403784439));
#16035=DIRECTION('',(0.5,0.,0.866025403784439));
#16036=DIRECTION('',(0.,-1.,0.));
#16037=DIRECTION('center_axis',(4.61511044732058E-15,0.,-1.));
#16038=DIRECTION('ref_axis',(1.,0.,4.61511044732058E-15));
#16039=DIRECTION('',(-1.,0.,-4.61511044732058E-15));
#16040=DIRECTION('',(1.,0.,4.61511044732058E-15));
#16041=DIRECTION('center_axis',(0.,1.,0.));
#16042=DIRECTION('ref_axis',(-1.,0.,0.));
#16043=DIRECTION('center_axis',(0.,1.,0.));
#16044=DIRECTION('ref_axis',(-1.,0.,0.));
#16045=DIRECTION('',(0.,0.,1.));
#16046=DIRECTION('',(1.,0.,0.));
#16047=DIRECTION('',(0.,0.,1.));
#16048=DIRECTION('',(1.,0.,0.));
#16049=DIRECTION('',(0.,0.,1.));
#16050=DIRECTION('',(1.,0.,0.));
#16051=DIRECTION('',(0.,0.,1.));
#16052=DIRECTION('',(1.,0.,0.));
#16053=DIRECTION('',(0.,0.,1.));
#16054=DIRECTION('',(1.,0.,0.));
#16055=DIRECTION('',(0.,0.,1.));
#16056=DIRECTION('',(1.,0.,0.));
#16057=DIRECTION('',(0.,0.,1.));
#16058=DIRECTION('',(1.,0.,0.));
#16059=DIRECTION('',(0.,0.,1.));
#16060=DIRECTION('',(1.,0.,0.));
#16061=DIRECTION('',(0.,0.,1.));
#16062=DIRECTION('',(1.,0.,0.));
#16063=DIRECTION('',(0.,0.,1.));
#16064=DIRECTION('',(1.,0.,0.));
#16065=DIRECTION('',(0.,0.,1.));
#16066=DIRECTION('',(1.,0.,0.));
#16067=DIRECTION('',(0.,0.,1.));
#16068=DIRECTION('',(1.,0.,0.));
#16069=DIRECTION('',(0.,0.,1.));
#16070=DIRECTION('',(1.,0.,0.));
#16071=DIRECTION('',(0.,0.,1.));
#16072=DIRECTION('',(1.,0.,0.));
#16073=CARTESIAN_POINT('',(0.,0.,0.));
#16074=CARTESIAN_POINT('',(0.,0.,0.));
#16075=CARTESIAN_POINT('Origin',(24.1201056133058,-79.5,35.8480593298244));
#16076=CARTESIAN_POINT('',(24.1201056133058,-80.,56.5961186596487));
#16077=CARTESIAN_POINT('Origin',(24.1201056133058,-80.,35.8480593298244));
#16078=CARTESIAN_POINT('',(24.1201056133058,-79.5,57.0961186596487));
#16079=CARTESIAN_POINT('Origin',(24.1201056133058,-79.5,56.5961186596487));
#16080=CARTESIAN_POINT('',(2.87204628348146,-79.5,35.8480593298243));
#16081=CARTESIAN_POINT('Origin',(24.1201056133058,-79.5,35.8480593298244));
#16082=CARTESIAN_POINT('Origin',(24.1201056133058,-79.5,35.8480593298244));
#16083=CARTESIAN_POINT('Origin',(24.1201056133058,-55.,35.8480593298244));
#16084=CARTESIAN_POINT('',(2.87204628348146,-55.5,35.8480593298244));
#16085=CARTESIAN_POINT('',(2.87204628348146,-55.,35.8480593298243));
#16086=CARTESIAN_POINT('',(24.1201056133058,-55.5,57.0961186596487));
#16087=CARTESIAN_POINT('Origin',(24.1201056133058,-55.5,35.8480593298244));
#16088=CARTESIAN_POINT('Origin',(24.1201056133058,-55.5,35.8480593298244));
#16089=CARTESIAN_POINT('Origin',(24.1201056133058,-80.,35.8480593298243));
#16090=CARTESIAN_POINT('Origin',(24.1201056133058,-55.5,35.8480593298244));
#16091=CARTESIAN_POINT('',(24.1201056133058,-55.,56.5961186596487));
#16092=CARTESIAN_POINT('Origin',(24.1201056133058,-55.5,56.5961186596487));
#16093=CARTESIAN_POINT('Origin',(24.1201056133058,-55.,35.8480593298244));
#16094=CARTESIAN_POINT('Origin',(24.1201056133058,4.5,35.8480593298244));
#16095=CARTESIAN_POINT('',(2.87204628348146,4.5,35.8480593298244));
#16096=CARTESIAN_POINT('',(24.1201056133058,4.5,57.0961186596487));
#16097=CARTESIAN_POINT('Origin',(24.1201056133058,4.5,35.8480593298244));
#16098=CARTESIAN_POINT('',(24.1201056133058,5.,56.5961186596487));
#16099=CARTESIAN_POINT('Origin',(24.1201056133058,4.5,56.5961186596487));
#16100=CARTESIAN_POINT('Origin',(24.1201056133058,5.,35.8480593298244));
#16101=CARTESIAN_POINT('Origin',(24.1201056133058,4.5,35.8480593298244));
#16102=CARTESIAN_POINT('Origin',(24.1201056133058,5.,35.8480593298244));
#16103=CARTESIAN_POINT('',(2.87204628348146,-54.5,35.8480593298243));
#16104=CARTESIAN_POINT('',(24.1201056133058,-54.5,57.0961186596487));
#16105=CARTESIAN_POINT('Origin',(24.1201056133058,-54.5,35.8480593298244));
#16106=CARTESIAN_POINT('',(2.87204628348146,5.,35.8480593298243));
#16107=CARTESIAN_POINT('Origin',(24.1201056133058,-54.5,35.8480593298244));
#16108=CARTESIAN_POINT('Origin',(24.1201056133058,-54.5,35.8480593298244));
#16109=CARTESIAN_POINT('Origin',(24.1201056133058,-54.5,56.5961186596487));
#16110=CARTESIAN_POINT('Origin',(24.1201056133058,65.999994278,35.8480593298244));
#16111=CARTESIAN_POINT('',(30.1201056133058,65.999994278,35.8480593298244));
#16112=CARTESIAN_POINT('Origin',(24.1201056133058,65.999994278,35.8480593298244));
#16113=CARTESIAN_POINT('Origin',(24.1201056133058,45.,35.8480593298244));
#16114=CARTESIAN_POINT('',(30.1201056133058,45.,35.8480593298244));
#16115=CARTESIAN_POINT('',(30.1201056133058,45.,35.8480593298244));
#16116=CARTESIAN_POINT('Origin',(24.1201056133058,45.,35.8480593298244));
#16117=CARTESIAN_POINT('Origin',(24.1201056133058,44.5,35.8480593298244));
#16118=CARTESIAN_POINT('',(24.1201056133058,45.,15.1));
#16119=CARTESIAN_POINT('Origin',(24.1201056133058,45.,35.8480593298244));
#16120=CARTESIAN_POINT('',(24.1201056133058,44.5,14.6));
#16121=CARTESIAN_POINT('Origin',(24.1201056133058,44.5,15.1));
#16122=CARTESIAN_POINT('',(2.87204628348146,44.5,35.8480593298244));
#16123=CARTESIAN_POINT('Origin',(24.1201056133058,44.5,35.8480593298244));
#16124=CARTESIAN_POINT('Origin',(24.1201056133058,44.5,35.8480593298244));
#16125=CARTESIAN_POINT('Origin',(24.1201056133058,25.,35.8480593298244));
#16126=CARTESIAN_POINT('',(2.87204628348146,5.5,35.8480593298243));
#16127=CARTESIAN_POINT('',(2.87204628348146,25.,35.8480593298244));
#16128=CARTESIAN_POINT('',(24.1201056133058,5.5,57.0961186596487));
#16129=CARTESIAN_POINT('Origin',(24.1201056133058,5.5,35.8480593298244));
#16130=CARTESIAN_POINT('Origin',(24.1201056133058,5.5,35.8480593298244));
#16131=CARTESIAN_POINT('Origin',(24.1201056133058,45.,35.8480593298243));
#16132=CARTESIAN_POINT('Origin',(24.1201056133058,5.5,35.8480593298244));
#16133=CARTESIAN_POINT('Origin',(24.1201056133058,5.5,56.5961186596487));
#16134=CARTESIAN_POINT('',(0.,0.,0.));
#16135=CARTESIAN_POINT('Origin',(24.1201056133058,58.,35.8480593298244));
#16136=CARTESIAN_POINT('',(44.8681649431302,58.,35.8480593298243));
#16137=CARTESIAN_POINT('Origin',(24.1201056133058,58.,35.8480593298244));
#16138=CARTESIAN_POINT('',(40.8681649431302,58.,35.8480593298244));
#16139=CARTESIAN_POINT('Origin',(24.1201056133058,58.,35.8480593298244));
#16140=CARTESIAN_POINT('Origin',(24.1201056133058,57.,35.8480593298244));
#16141=CARTESIAN_POINT('',(44.8681649431302,57.,35.8480593298243));
#16142=CARTESIAN_POINT('',(44.8681649431302,57.,35.8480593298243));
#16143=CARTESIAN_POINT('Origin',(24.1201056133058,57.,35.8480593298244));
#16144=CARTESIAN_POINT('Origin',(24.1201056133058,57.,35.8480593298244));
#16145=CARTESIAN_POINT('',(39.8681649431302,57.,35.8480593298244));
#16146=CARTESIAN_POINT('Origin',(24.1201056133058,57.,35.8480593298244));
#16147=CARTESIAN_POINT('Origin',(24.1201056133058,66.,35.8480593298244));
#16148=CARTESIAN_POINT('',(44.8681649431302,66.,35.8480593298243));
#16149=CARTESIAN_POINT('Origin',(24.1201056133058,66.,35.8480593298244));
#16150=CARTESIAN_POINT('',(40.8681649431302,66.,35.8480593298244));
#16151=CARTESIAN_POINT('Origin',(24.1201056133058,66.,35.8480593298244));
#16152=CARTESIAN_POINT('Origin',(24.1201056133058,65.,35.8480593298244));
#16153=CARTESIAN_POINT('',(44.8681649431302,65.,35.8480593298243));
#16154=CARTESIAN_POINT('Origin',(24.1201056133058,65.,35.8480593298244));
#16155=CARTESIAN_POINT('',(40.8681649431302,65.,35.8480593298244));
#16156=CARTESIAN_POINT('Origin',(24.1201056133058,65.,35.8480593298244));
#16157=CARTESIAN_POINT('Origin',(24.1201056133058,65.,35.8480593298244));
#16158=CARTESIAN_POINT('',(44.8681649431302,65.,35.8480593298243));
#16159=CARTESIAN_POINT('Origin',(24.1201056133058,72.,35.8480593298244));
#16160=CARTESIAN_POINT('',(40.8681649431302,72.,35.8480593298244));
#16161=CARTESIAN_POINT('Origin',(24.1201056133058,72.,35.8480593298244));
#16162=CARTESIAN_POINT('',(44.8681649431302,72.,35.8480593298243));
#16163=CARTESIAN_POINT('Origin',(24.1201056133058,72.,35.8480593298244));
#16164=CARTESIAN_POINT('',(40.8681649431302,72.,35.8480593298244));
#16165=CARTESIAN_POINT('Origin',(24.1201056133058,72.,35.8480593298244));
#16166=CARTESIAN_POINT('Origin',(24.1201056133058,72.,35.8480593298244));
#16167=CARTESIAN_POINT('',(44.8681649431302,73.,35.8480593298243));
#16168=CARTESIAN_POINT('Origin',(24.1201056133058,73.,35.8480593298244));
#16169=CARTESIAN_POINT('',(44.8681649431302,72.,35.8480593298243));
#16170=CARTESIAN_POINT('Origin',(24.1201056133058,73.,35.8480593298244));
#16171=CARTESIAN_POINT('',(39.8681649431302,73.,35.8480593298244));
#16172=CARTESIAN_POINT('Origin',(24.1201056133058,73.,35.8480593298244));
#16173=CARTESIAN_POINT('Origin',(24.1201056133058,72.,35.8480593298244));
#16174=CARTESIAN_POINT('',(39.8681649431302,65.,35.8480593298244));
#16175=CARTESIAN_POINT('',(39.8681649431302,72.,35.8480593298244));
#16176=CARTESIAN_POINT('Origin',(24.1201056133058,65.,35.8480593298244));
#16177=CARTESIAN_POINT('Origin',(24.1201056133058,72.,35.8480593298244));
#16178=CARTESIAN_POINT('',(39.8681649431302,66.,35.8480593298244));
#16179=CARTESIAN_POINT('Origin',(24.1201056133058,66.,35.8480593298244));
#16180=CARTESIAN_POINT('',(39.8681649431302,72.,35.8480593298244));
#16181=CARTESIAN_POINT('Origin',(24.1201056133058,72.,35.8480593298244));
#16182=CARTESIAN_POINT('',(40.8681649431302,72.,35.8480593298244));
#16183=CARTESIAN_POINT('Origin',(24.1201056133058,66.,35.8480593298244));
#16184=CARTESIAN_POINT('',(30.1201056133058,66.,35.8480593298244));
#16185=CARTESIAN_POINT('Origin',(24.1201056133058,66.,35.8480593298244));
#16186=CARTESIAN_POINT('Origin',(24.1201056133058,72.,35.8480593298244));
#16187=CARTESIAN_POINT('',(30.1201056133058,65.,35.8480593298244));
#16188=CARTESIAN_POINT('Origin',(24.1201056133058,65.,35.8480593298244));
#16189=CARTESIAN_POINT('',(30.1201056133058,72.,35.8480593298244));
#16190=CARTESIAN_POINT('Origin',(24.1201056133058,65.,35.8480593298244));
#16191=CARTESIAN_POINT('',(0.,0.,0.));
#16192=CARTESIAN_POINT('Origin',(1.,0.,13.));
#16193=CARTESIAN_POINT('',(0.,50.,13.));
#16194=CARTESIAN_POINT('',(1.,50.,12.));
#16195=CARTESIAN_POINT('Origin',(1.,50.,13.));
#16196=CARTESIAN_POINT('',(1.,0.,12.));
#16197=CARTESIAN_POINT('',(1.,0.,12.));
#16198=CARTESIAN_POINT('',(0.,0.,13.));
#16199=CARTESIAN_POINT('Origin',(1.,0.,13.));
#16200=CARTESIAN_POINT('',(0.,0.,13.));
#16201=CARTESIAN_POINT('Origin',(0.,0.,12.));
#16202=CARTESIAN_POINT('',(0.,0.,58.9890118784622));
#16203=CARTESIAN_POINT('',(0.,0.,59.9890118784622));
#16204=CARTESIAN_POINT('',(0.,50.,58.9890118784622));
#16205=CARTESIAN_POINT('',(0.,0.,58.9890118784622));
#16206=CARTESIAN_POINT('',(0.,50.,59.9890118784622));
#16207=CARTESIAN_POINT('',(0.,30.9806853933445,48.4577900798939));
#16208=CARTESIAN_POINT('Origin',(-8.65036710704234E-15,30.9806853933445,
50.9577900798939));
#16209=CARTESIAN_POINT('',(-8.88178419700125E-15,30.9806853933445,17.4577900798938));
#16210=CARTESIAN_POINT('Origin',(-1.76698435436636E-15,30.9806853933445,
19.9577900798938));
#16211=CARTESIAN_POINT('',(-8.88178419700125E-15,42.6473520600112,32.9577900798939));
#16212=CARTESIAN_POINT('Origin',(-5.20867573070435E-15,42.6473520600112,
35.4577900798939));
#16213=CARTESIAN_POINT('',(-8.88178419700125E-15,25.,28.515352874563));
#16214=CARTESIAN_POINT('Origin',(-5.33247954116756E-15,25.,36.015352874563));
#16215=CARTESIAN_POINT('',(0.,7.64735206001121,48.4577900798939));
#16216=CARTESIAN_POINT('Origin',(-8.65036710704234E-15,7.64735206001121,
50.9577900798939));
#16217=CARTESIAN_POINT('',(-8.88178419700125E-15,7.64735206001121,17.4577900798938));
#16218=CARTESIAN_POINT('Origin',(-1.76698435436636E-15,7.64735206001121,
19.9577900798938));
#16219=CARTESIAN_POINT('',(-8.88178419700125E-15,7.64735206001121,32.9577900798939));
#16220=CARTESIAN_POINT('Origin',(-5.20867573070435E-15,7.64735206001121,
35.4577900798939));
#16221=CARTESIAN_POINT('',(0.,42.6473520600112,48.4577900798939));
#16222=CARTESIAN_POINT('Origin',(-8.65036710704234E-15,42.6473520600112,
50.9577900798939));
#16223=CARTESIAN_POINT('',(-8.88178419700125E-15,42.6473520600112,17.4577900798938));
#16224=CARTESIAN_POINT('Origin',(-1.76698435436636E-15,42.6473520600112,
19.9577900798938));
#16225=CARTESIAN_POINT('',(0.,19.3140187266779,48.4577900798939));
#16226=CARTESIAN_POINT('Origin',(-8.65036710704234E-15,19.3140187266779,
50.9577900798939));
#16227=CARTESIAN_POINT('',(-8.88178419700125E-15,19.3140187266779,17.4577900798938));
#16228=CARTESIAN_POINT('Origin',(-1.76698435436636E-15,19.3140187266779,
19.9577900798938));
#16229=CARTESIAN_POINT('Origin',(23.9736590038991,0.,35.9945059392311));
#16230=CARTESIAN_POINT('',(47.9473180077982,0.,12.));
#16231=CARTESIAN_POINT('',(0.,0.,12.));
#16232=CARTESIAN_POINT('',(47.9473180077982,0.,14.6));
#16233=CARTESIAN_POINT('',(47.9473180077982,0.,12.));
#16234=CARTESIAN_POINT('',(2.6,0.,14.6));
#16235=CARTESIAN_POINT('',(2.6,0.,14.6));
#16236=CARTESIAN_POINT('',(2.6,0.,57.3890118784622));
#16237=CARTESIAN_POINT('',(2.6,0.,57.3890118784622));
#16238=CARTESIAN_POINT('',(47.9473180077982,0.,57.3890118784622));
#16239=CARTESIAN_POINT('',(47.9473180077982,0.,57.3890118784622));
#16240=CARTESIAN_POINT('',(47.9473180077982,0.,59.9890118784622));
#16241=CARTESIAN_POINT('',(47.9473180077982,0.,12.));
#16242=CARTESIAN_POINT('',(0.999999999999996,0.,59.9890118784622));
#16243=CARTESIAN_POINT('',(47.9473180077982,0.,59.9890118784622));
#16244=CARTESIAN_POINT('Origin',(1.,0.,58.9890118784622));
#16245=CARTESIAN_POINT('Origin',(1.,0.,58.9890118784622));
#16246=CARTESIAN_POINT('',(0.999999999999996,50.,59.9890118784622));
#16247=CARTESIAN_POINT('Origin',(1.,50.,58.9890118784622));
#16248=CARTESIAN_POINT('',(1.,0.,59.9890118784622));
#16249=CARTESIAN_POINT('Origin',(9.03122179856829,19.3140187266779,59.9890118784622));
#16250=CARTESIAN_POINT('',(11.5312217985683,19.3140187266779,14.6));
#16251=CARTESIAN_POINT('Origin',(9.03122179856829,19.3140187266779,14.6));
#16252=CARTESIAN_POINT('',(11.5312217985683,19.3140187266779,12.));
#16253=CARTESIAN_POINT('',(11.5312217985683,19.3140187266779,59.9890118784622));
#16254=CARTESIAN_POINT('Origin',(9.03122179856829,19.3140187266779,12.));
#16255=CARTESIAN_POINT('Origin',(9.03122179856829,30.9806853933445,59.9890118784622));
#16256=CARTESIAN_POINT('',(11.5312217985683,30.9806853933445,14.6));
#16257=CARTESIAN_POINT('Origin',(9.03122179856829,30.9806853933445,14.6));
#16258=CARTESIAN_POINT('',(11.5312217985683,30.9806853933445,12.));
#16259=CARTESIAN_POINT('',(11.5312217985683,30.9806853933445,59.9890118784622));
#16260=CARTESIAN_POINT('Origin',(9.03122179856829,30.9806853933445,12.));
#16261=CARTESIAN_POINT('Origin',(9.03122179856829,42.6473520600112,59.9890118784622));
#16262=CARTESIAN_POINT('',(11.5312217985683,42.6473520600112,14.6));
#16263=CARTESIAN_POINT('Origin',(9.03122179856829,42.6473520600112,14.6));
#16264=CARTESIAN_POINT('',(11.5312217985683,42.6473520600112,12.));
#16265=CARTESIAN_POINT('',(11.5312217985683,42.6473520600112,59.9890118784622));
#16266=CARTESIAN_POINT('Origin',(9.03122179856829,42.6473520600112,12.));
#16267=CARTESIAN_POINT('Origin',(23.9736590038991,25.,59.9890118784622));
#16268=CARTESIAN_POINT('',(31.4736590038991,25.,14.6));
#16269=CARTESIAN_POINT('Origin',(23.9736590038991,25.,14.6));
#16270=CARTESIAN_POINT('',(31.4736590038991,25.,12.));
#16271=CARTESIAN_POINT('',(31.4736590038991,25.,59.9890118784622));
#16272=CARTESIAN_POINT('Origin',(23.9736590038991,25.,12.));
#16273=CARTESIAN_POINT('Origin',(40.0312217985683,30.9806853933445,59.9890118784622));
#16274=CARTESIAN_POINT('',(42.5312217985683,30.9806853933445,14.6));
#16275=CARTESIAN_POINT('Origin',(40.0312217985683,30.9806853933445,14.6));
#16276=CARTESIAN_POINT('',(42.5312217985683,30.9806853933445,12.));
#16277=CARTESIAN_POINT('',(42.5312217985683,30.9806853933445,59.9890118784622));
#16278=CARTESIAN_POINT('Origin',(40.0312217985683,30.9806853933445,12.));
#16279=CARTESIAN_POINT('Origin',(40.0312217985683,19.3140187266779,59.9890118784622));
#16280=CARTESIAN_POINT('',(42.5312217985683,19.3140187266779,14.6));
#16281=CARTESIAN_POINT('Origin',(40.0312217985683,19.3140187266779,14.6));
#16282=CARTESIAN_POINT('',(42.5312217985683,19.3140187266779,12.));
#16283=CARTESIAN_POINT('',(42.5312217985683,19.3140187266779,59.9890118784622));
#16284=CARTESIAN_POINT('Origin',(40.0312217985683,19.3140187266779,12.));
#16285=CARTESIAN_POINT('Origin',(40.0312217985683,7.64735206001121,59.9890118784622));
#16286=CARTESIAN_POINT('',(42.5312217985683,7.64735206001121,14.6));
#16287=CARTESIAN_POINT('Origin',(40.0312217985683,7.64735206001121,14.6));
#16288=CARTESIAN_POINT('',(42.5312217985683,7.64735206001121,12.));
#16289=CARTESIAN_POINT('',(42.5312217985683,7.64735206001121,59.9890118784622));
#16290=CARTESIAN_POINT('Origin',(40.0312217985683,7.64735206001121,12.));
#16291=CARTESIAN_POINT('Origin',(24.5312217985683,42.6473520600112,59.9890118784622));
#16292=CARTESIAN_POINT('',(27.0312217985683,42.6473520600112,14.6));
#16293=CARTESIAN_POINT('Origin',(24.5312217985683,42.6473520600112,14.6));
#16294=CARTESIAN_POINT('',(27.0312217985683,42.6473520600112,12.));
#16295=CARTESIAN_POINT('',(27.0312217985683,42.6473520600112,59.9890118784622));
#16296=CARTESIAN_POINT('Origin',(24.5312217985683,42.6473520600112,12.));
#16297=CARTESIAN_POINT('Origin',(40.0312217985683,42.6473520600112,59.9890118784622));
#16298=CARTESIAN_POINT('',(42.5312217985683,42.6473520600112,14.6));
#16299=CARTESIAN_POINT('Origin',(40.0312217985683,42.6473520600112,14.6));
#16300=CARTESIAN_POINT('',(42.5312217985683,42.6473520600112,12.));
#16301=CARTESIAN_POINT('',(42.5312217985683,42.6473520600112,59.9890118784622));
#16302=CARTESIAN_POINT('Origin',(40.0312217985683,42.6473520600112,12.));
#16303=CARTESIAN_POINT('Origin',(24.5312217985683,7.64735206001121,59.9890118784622));
#16304=CARTESIAN_POINT('',(27.0312217985683,7.64735206001121,14.6));
#16305=CARTESIAN_POINT('Origin',(24.5312217985683,7.64735206001121,14.6));
#16306=CARTESIAN_POINT('',(27.0312217985683,7.64735206001121,12.));
#16307=CARTESIAN_POINT('',(27.0312217985683,7.64735206001121,59.9890118784622));
#16308=CARTESIAN_POINT('Origin',(24.5312217985683,7.64735206001121,12.));
#16309=CARTESIAN_POINT('Origin',(9.03122179856829,7.64735206001121,59.9890118784622));
#16310=CARTESIAN_POINT('',(11.5312217985683,7.64735206001121,14.6));
#16311=CARTESIAN_POINT('Origin',(9.03122179856829,7.64735206001121,14.6));
#16312=CARTESIAN_POINT('',(11.5312217985683,7.64735206001121,12.));
#16313=CARTESIAN_POINT('',(11.5312217985683,7.64735206001121,59.9890118784622));
#16314=CARTESIAN_POINT('Origin',(9.03122179856829,7.64735206001121,12.));
#16315=CARTESIAN_POINT('Origin',(-8.88178419700125E-15,19.3140187266779,
19.9577900798938));
#16316=CARTESIAN_POINT('',(2.60000000000001,19.3140187266779,17.4577900798939));
#16317=CARTESIAN_POINT('',(-9.43689570931383E-15,19.3140187266779,17.4577900798939));
#16318=CARTESIAN_POINT('Origin',(2.60000000000001,19.3140187266779,19.9577900798938));
#16319=CARTESIAN_POINT('Origin',(0.,19.3140187266779,50.9577900798939));
#16320=CARTESIAN_POINT('',(2.6,19.3140187266779,48.4577900798939));
#16321=CARTESIAN_POINT('',(-5.55111512312577E-16,19.3140187266779,48.4577900798939));
#16322=CARTESIAN_POINT('Origin',(2.6,19.3140187266779,50.9577900798939));
#16323=CARTESIAN_POINT('Origin',(-8.88178419700125E-15,42.6473520600112,
19.9577900798938));
#16324=CARTESIAN_POINT('',(2.60000000000001,42.6473520600112,17.4577900798939));
#16325=CARTESIAN_POINT('',(-9.43689570931383E-15,42.6473520600112,17.4577900798939));
#16326=CARTESIAN_POINT('Origin',(2.60000000000001,42.6473520600112,19.9577900798938));
#16327=CARTESIAN_POINT('Origin',(0.,42.6473520600112,50.9577900798939));
#16328=CARTESIAN_POINT('',(2.6,42.6473520600112,48.4577900798939));
#16329=CARTESIAN_POINT('',(-5.55111512312577E-16,42.6473520600112,48.4577900798939));
#16330=CARTESIAN_POINT('Origin',(2.6,42.6473520600112,50.9577900798939));
#16331=CARTESIAN_POINT('Origin',(-8.88178419700125E-15,7.64735206001121,
35.4577900798939));
#16332=CARTESIAN_POINT('',(2.6,7.64735206001121,32.9577900798939));
#16333=CARTESIAN_POINT('',(-9.43689570931383E-15,7.64735206001121,32.9577900798939));
#16334=CARTESIAN_POINT('Origin',(2.6,7.64735206001121,35.4577900798939));
#16335=CARTESIAN_POINT('Origin',(-8.88178419700125E-15,7.64735206001121,
19.9577900798938));
#16336=CARTESIAN_POINT('',(2.60000000000001,7.64735206001121,17.4577900798939));
#16337=CARTESIAN_POINT('',(-9.43689570931383E-15,7.64735206001121,17.4577900798939));
#16338=CARTESIAN_POINT('Origin',(2.60000000000001,7.64735206001121,19.9577900798938));
#16339=CARTESIAN_POINT('Origin',(0.,7.64735206001121,50.9577900798939));
#16340=CARTESIAN_POINT('',(2.6,7.64735206001121,48.4577900798939));
#16341=CARTESIAN_POINT('',(-5.55111512312577E-16,7.64735206001121,48.4577900798939));
#16342=CARTESIAN_POINT('Origin',(2.6,7.64735206001121,50.9577900798939));
#16343=CARTESIAN_POINT('Origin',(-8.88178419700125E-15,25.,36.015352874563));
#16344=CARTESIAN_POINT('',(2.6,25.,28.515352874563));
#16345=CARTESIAN_POINT('',(-1.0547118733939E-14,25.,28.515352874563));
#16346=CARTESIAN_POINT('Origin',(2.6,25.,36.015352874563));
#16347=CARTESIAN_POINT('Origin',(-8.88178419700125E-15,42.6473520600112,
35.4577900798939));
#16348=CARTESIAN_POINT('',(2.6,42.6473520600112,32.9577900798939));
#16349=CARTESIAN_POINT('',(-9.43689570931383E-15,42.6473520600112,32.9577900798939));
#16350=CARTESIAN_POINT('Origin',(2.6,42.6473520600112,35.4577900798939));
#16351=CARTESIAN_POINT('Origin',(-8.88178419700125E-15,30.9806853933445,
19.9577900798938));
#16352=CARTESIAN_POINT('',(2.60000000000001,30.9806853933445,17.4577900798939));
#16353=CARTESIAN_POINT('',(-9.43689570931383E-15,30.9806853933445,17.4577900798939));
#16354=CARTESIAN_POINT('Origin',(2.60000000000001,30.9806853933445,19.9577900798938));
#16355=CARTESIAN_POINT('Origin',(0.,30.9806853933445,50.9577900798939));
#16356=CARTESIAN_POINT('',(2.6,30.9806853933445,48.4577900798939));
#16357=CARTESIAN_POINT('',(-5.55111512312577E-16,30.9806853933445,48.4577900798939));
#16358=CARTESIAN_POINT('Origin',(2.6,30.9806853933445,50.9577900798939));
#16359=CARTESIAN_POINT('Origin',(9.03122179856829,19.3140187266779,59.9890118784622));
#16360=CARTESIAN_POINT('',(11.5312217985683,19.3140187266779,59.9890118784622));
#16361=CARTESIAN_POINT('Origin',(9.03122179856829,19.3140187266779,59.9890118784622));
#16362=CARTESIAN_POINT('',(11.5312217985683,19.3140187266779,57.3890118784622));
#16363=CARTESIAN_POINT('',(11.5312217985683,19.3140187266779,59.9890118784622));
#16364=CARTESIAN_POINT('Origin',(9.03122179856829,19.3140187266779,57.3890118784622));
#16365=CARTESIAN_POINT('Origin',(9.03122179856829,42.6473520600112,59.9890118784622));
#16366=CARTESIAN_POINT('',(11.5312217985683,42.6473520600112,59.9890118784622));
#16367=CARTESIAN_POINT('Origin',(9.03122179856829,42.6473520600112,59.9890118784622));
#16368=CARTESIAN_POINT('',(11.5312217985683,42.6473520600112,57.3890118784622));
#16369=CARTESIAN_POINT('',(11.5312217985683,42.6473520600112,59.9890118784622));
#16370=CARTESIAN_POINT('Origin',(9.03122179856829,42.6473520600112,57.3890118784622));
#16371=CARTESIAN_POINT('Origin',(40.0312217985683,7.64735206001121,59.9890118784622));
#16372=CARTESIAN_POINT('',(42.5312217985683,7.64735206001121,59.9890118784622));
#16373=CARTESIAN_POINT('Origin',(40.0312217985683,7.64735206001121,59.9890118784622));
#16374=CARTESIAN_POINT('',(42.5312217985683,7.64735206001121,57.3890118784622));
#16375=CARTESIAN_POINT('',(42.5312217985683,7.64735206001121,59.9890118784622));
#16376=CARTESIAN_POINT('Origin',(40.0312217985683,7.64735206001121,57.3890118784622));
#16377=CARTESIAN_POINT('Origin',(23.9736590038991,25.,59.9890118784622));
#16378=CARTESIAN_POINT('',(31.4736590038991,25.,59.9890118784622));
#16379=CARTESIAN_POINT('Origin',(23.9736590038991,25.,59.9890118784622));
#16380=CARTESIAN_POINT('',(31.4736590038991,25.,57.3890118784622));
#16381=CARTESIAN_POINT('',(31.4736590038991,25.,59.9890118784622));
#16382=CARTESIAN_POINT('Origin',(23.9736590038991,25.,57.3890118784622));
#16383=CARTESIAN_POINT('Origin',(40.0312217985683,30.9806853933445,59.9890118784622));
#16384=CARTESIAN_POINT('',(42.5312217985683,30.9806853933445,59.9890118784622));
#16385=CARTESIAN_POINT('Origin',(40.0312217985683,30.9806853933445,59.9890118784622));
#16386=CARTESIAN_POINT('',(42.5312217985683,30.9806853933445,57.3890118784622));
#16387=CARTESIAN_POINT('',(42.5312217985683,30.9806853933445,59.9890118784622));
#16388=CARTESIAN_POINT('Origin',(40.0312217985683,30.9806853933445,57.3890118784622));
#16389=CARTESIAN_POINT('Origin',(9.03122179856829,30.9806853933445,59.9890118784622));
#16390=CARTESIAN_POINT('',(11.5312217985683,30.9806853933445,59.9890118784622));
#16391=CARTESIAN_POINT('Origin',(9.03122179856829,30.9806853933445,59.9890118784622));
#16392=CARTESIAN_POINT('',(11.5312217985683,30.9806853933445,57.3890118784622));
#16393=CARTESIAN_POINT('',(11.5312217985683,30.9806853933445,59.9890118784622));
#16394=CARTESIAN_POINT('Origin',(9.03122179856829,30.9806853933445,57.3890118784622));
#16395=CARTESIAN_POINT('Origin',(24.5312217985683,42.6473520600112,59.9890118784622));
#16396=CARTESIAN_POINT('',(27.0312217985683,42.6473520600112,59.9890118784622));
#16397=CARTESIAN_POINT('Origin',(24.5312217985683,42.6473520600112,59.9890118784622));
#16398=CARTESIAN_POINT('',(27.0312217985683,42.6473520600112,57.3890118784622));
#16399=CARTESIAN_POINT('',(27.0312217985683,42.6473520600112,59.9890118784622));
#16400=CARTESIAN_POINT('Origin',(24.5312217985683,42.6473520600112,57.3890118784622));
#16401=CARTESIAN_POINT('Origin',(9.03122179856829,7.64735206001121,59.9890118784622));
#16402=CARTESIAN_POINT('',(11.5312217985683,7.64735206001121,59.9890118784622));
#16403=CARTESIAN_POINT('Origin',(9.03122179856829,7.64735206001121,59.9890118784622));
#16404=CARTESIAN_POINT('',(11.5312217985683,7.64735206001121,57.3890118784622));
#16405=CARTESIAN_POINT('',(11.5312217985683,7.64735206001121,59.9890118784622));
#16406=CARTESIAN_POINT('Origin',(9.03122179856829,7.64735206001121,57.3890118784622));
#16407=CARTESIAN_POINT('Origin',(24.5312217985683,7.64735206001121,59.9890118784622));
#16408=CARTESIAN_POINT('',(27.0312217985683,7.64735206001121,59.9890118784622));
#16409=CARTESIAN_POINT('Origin',(24.5312217985683,7.64735206001121,59.9890118784622));
#16410=CARTESIAN_POINT('',(27.0312217985683,7.64735206001121,57.3890118784622));
#16411=CARTESIAN_POINT('',(27.0312217985683,7.64735206001121,59.9890118784622));
#16412=CARTESIAN_POINT('Origin',(24.5312217985683,7.64735206001121,57.3890118784622));
#16413=CARTESIAN_POINT('Origin',(40.0312217985683,42.6473520600112,59.9890118784622));
#16414=CARTESIAN_POINT('',(42.5312217985683,42.6473520600112,59.9890118784622));
#16415=CARTESIAN_POINT('Origin',(40.0312217985683,42.6473520600112,59.9890118784622));
#16416=CARTESIAN_POINT('',(42.5312217985683,42.6473520600112,57.3890118784622));
#16417=CARTESIAN_POINT('',(42.5312217985683,42.6473520600112,59.9890118784622));
#16418=CARTESIAN_POINT('Origin',(40.0312217985683,42.6473520600112,57.3890118784622));
#16419=CARTESIAN_POINT('Origin',(40.0312217985683,19.3140187266779,59.9890118784622));
#16420=CARTESIAN_POINT('',(42.5312217985683,19.3140187266779,59.9890118784622));
#16421=CARTESIAN_POINT('Origin',(40.0312217985683,19.3140187266779,59.9890118784622));
#16422=CARTESIAN_POINT('',(42.5312217985683,19.3140187266779,57.3890118784622));
#16423=CARTESIAN_POINT('',(42.5312217985683,19.3140187266779,59.9890118784622));
#16424=CARTESIAN_POINT('Origin',(40.0312217985683,19.3140187266779,57.3890118784622));
#16425=CARTESIAN_POINT('Origin',(47.9473180077982,0.,59.9890118784622));
#16426=CARTESIAN_POINT('',(47.9473180077982,50.,57.3890118784622));
#16427=CARTESIAN_POINT('',(47.9473180077982,0.,57.3890118784622));
#16428=CARTESIAN_POINT('',(47.9473180077982,50.,59.9890118784622));
#16429=CARTESIAN_POINT('',(47.9473180077982,50.,12.));
#16430=CARTESIAN_POINT('',(47.9473180077982,0.,59.9890118784622));
#16431=CARTESIAN_POINT('Origin',(0.,0.,59.9890118784622));
#16432=CARTESIAN_POINT('',(47.9473180077982,50.,59.9890118784622));
#16433=CARTESIAN_POINT('Origin',(47.9473180077982,0.,12.));
#16434=CARTESIAN_POINT('',(47.9473180077982,50.,12.));
#16435=CARTESIAN_POINT('',(0.,50.,12.));
#16436=CARTESIAN_POINT('',(47.9473180077982,0.,12.));
#16437=CARTESIAN_POINT('Origin',(47.9473180077982,0.,14.6));
#16438=CARTESIAN_POINT('',(47.9473180077982,50.,14.6));
#16439=CARTESIAN_POINT('',(47.9473180077982,50.,12.));
#16440=CARTESIAN_POINT('',(47.9473180077982,0.,14.6));
#16441=CARTESIAN_POINT('Origin',(2.6,0.,14.6));
#16442=CARTESIAN_POINT('',(2.6,50.,14.6));
#16443=CARTESIAN_POINT('',(2.6,50.,14.6));
#16444=CARTESIAN_POINT('',(2.6,0.,14.6));
#16445=CARTESIAN_POINT('Origin',(2.6,0.,57.3890118784622));
#16446=CARTESIAN_POINT('',(2.6,50.,57.3890118784622));
#16447=CARTESIAN_POINT('',(2.6,50.,57.3890118784622));
#16448=CARTESIAN_POINT('',(2.6,0.,57.3890118784622));
#16449=CARTESIAN_POINT('Origin',(47.9473180077982,0.,57.3890118784622));
#16450=CARTESIAN_POINT('',(47.9473180077982,50.,57.3890118784622));
#16451=CARTESIAN_POINT('Origin',(23.9736590038991,50.,35.9945059392311));
#16452=CARTESIAN_POINT('',(0.,0.,0.));
#16453=CARTESIAN_POINT('Origin',(363.987734179926,50.,25.7372649179816));
#16454=CARTESIAN_POINT('',(365.301833806237,50.,23.8381926430366));
#16455=CARTESIAN_POINT('',(366.289428826807,50.,25.9257724399974));
#16456=CARTESIAN_POINT('',(365.301833806237,50.,23.8381926430366));
#16457=CARTESIAN_POINT('',(363.000139159357,50.,23.6496851210208));
#16458=CARTESIAN_POINT('',(363.000139159357,50.,23.6496851210208));
#16459=CARTESIAN_POINT('',(361.686039533046,50.,25.5487573959657));
#16460=CARTESIAN_POINT('',(361.686039533046,50.,25.5487573959657));
#16461=CARTESIAN_POINT('',(362.673634553616,50.,27.6363371929265));
#16462=CARTESIAN_POINT('',(362.673634553616,50.,27.6363371929265));
#16463=CARTESIAN_POINT('',(364.975329200496,50.,27.8248447149424));
#16464=CARTESIAN_POINT('',(364.975329200496,50.,27.8248447149424));
#16465=CARTESIAN_POINT('',(366.289428826807,50.,25.9257724399974));
#16466=CARTESIAN_POINT('',(362.524234179926,50.,25.7372649179816));
#16467=CARTESIAN_POINT('Origin',(363.987734179926,50.,25.7372649179816));
#16468=CARTESIAN_POINT('Origin',(363.000139159357,50.,23.6496851210208));
#16469=CARTESIAN_POINT('',(365.301833806237,49.,23.8381926430366));
#16470=CARTESIAN_POINT('',(365.301833806237,50.,23.8381926430366));
#16471=CARTESIAN_POINT('',(363.000139159357,49.,23.6496851210208));
#16472=CARTESIAN_POINT('',(363.000139159357,49.,23.6496851210208));
#16473=CARTESIAN_POINT('',(363.000139159357,50.,23.6496851210208));
#16474=CARTESIAN_POINT('Origin',(361.686039533046,50.,25.5487573959657));
#16475=CARTESIAN_POINT('',(361.686039533046,49.,25.5487573959657));
#16476=CARTESIAN_POINT('',(361.686039533046,49.,25.5487573959657));
#16477=CARTESIAN_POINT('',(361.686039533046,50.,25.5487573959657));
#16478=CARTESIAN_POINT('Origin',(362.673634553616,50.,27.6363371929265));
#16479=CARTESIAN_POINT('',(362.673634553616,49.,27.6363371929265));
#16480=CARTESIAN_POINT('',(362.673634553616,49.,27.6363371929265));
#16481=CARTESIAN_POINT('',(362.673634553616,50.,27.6363371929265));
#16482=CARTESIAN_POINT('Origin',(364.975329200496,50.,27.8248447149424));
#16483=CARTESIAN_POINT('',(364.975329200496,49.,27.8248447149424));
#16484=CARTESIAN_POINT('',(364.975329200496,49.,27.8248447149424));
#16485=CARTESIAN_POINT('',(364.975329200496,50.,27.8248447149424));
#16486=CARTESIAN_POINT('Origin',(366.289428826807,50.,25.9257724399974));
#16487=CARTESIAN_POINT('',(366.289428826807,49.,25.9257724399974));
#16488=CARTESIAN_POINT('',(366.289428826807,49.,25.9257724399974));
#16489=CARTESIAN_POINT('',(366.289428826807,50.,25.9257724399974));
#16490=CARTESIAN_POINT('Origin',(365.301833806237,50.,23.8381926430366));
#16491=CARTESIAN_POINT('',(365.301833806237,49.,23.8381926430366));
#16492=CARTESIAN_POINT('Origin',(363.987734179926,49.,25.7372649179816));
#16493=CARTESIAN_POINT('Origin',(363.987734179926,50.,25.7372649179816));
#16494=CARTESIAN_POINT('',(362.524234179926,63.,25.7372649179816));
#16495=CARTESIAN_POINT('Origin',(363.987734179926,63.,25.7372649179816));
#16496=CARTESIAN_POINT('',(362.524234179926,50.,25.7372649179816));
#16497=CARTESIAN_POINT('Origin',(363.987734179926,63.,25.7372649179816));
#16498=CARTESIAN_POINT('',(0.,0.,0.));
#16499=CARTESIAN_POINT('Origin',(384.,29.4811336906747,16.5456750096756));
#16500=CARTESIAN_POINT('',(384.,29.8952421751416,18.8877073880428));
#16501=CARTESIAN_POINT('',(384.,29.4811336906747,16.5456750096756));
#16502=CARTESIAN_POINT('',(384.,29.8952421751416,18.8877073880428));
#16503=CARTESIAN_POINT('',(47.9470000000001,29.4811336906747,16.5456750096756));
#16504=CARTESIAN_POINT('',(384.,29.4811336906747,16.5456750096756));
#16505=CARTESIAN_POINT('',(47.9470000000001,29.8952421751416,18.8877073880428));
#16506=CARTESIAN_POINT('',(47.9470000000001,29.8952421751416,18.8877073880428));
#16507=CARTESIAN_POINT('',(384.,29.8952421751416,18.8877073880428));
#16508=CARTESIAN_POINT('Origin',(384.,30.465859005635,16.3715599497981));
#16509=CARTESIAN_POINT('',(384.,29.643945736254,15.8019472940264));
#16510=CARTESIAN_POINT('Origin',(384.,30.465859005635,16.3715599497981));
#16511=CARTESIAN_POINT('',(47.9470000000001,29.643945736254,15.8019472940264));
#16512=CARTESIAN_POINT('',(384.,29.643945736254,15.8019472940264));
#16513=CARTESIAN_POINT('Origin',(47.9470000000001,30.465859005635,16.3715599497981));
#16514=CARTESIAN_POINT('Origin',(384.,31.5857864376269,13.));
#16515=CARTESIAN_POINT('',(384.,31.5857864376269,13.));
#16516=CARTESIAN_POINT('',(384.,29.643945736254,15.8019472940264));
#16517=CARTESIAN_POINT('',(47.9470000000001,31.5857864376269,13.));
#16518=CARTESIAN_POINT('',(384.,31.5857864376269,13.));
#16519=CARTESIAN_POINT('',(47.9470000000001,29.643945736254,15.8019472940264));
#16520=CARTESIAN_POINT('Origin',(384.,28.8220324668729,15.2323346382546));
#16521=CARTESIAN_POINT('',(384.,28.8220324668729,15.2323346382546));
#16522=CARTESIAN_POINT('',(384.,30.369113052182,13.));
#16523=CARTESIAN_POINT('',(384.,28.8220324668729,15.2323346382546));
#16524=CARTESIAN_POINT('',(47.9470000000001,28.8220324668729,15.2323346382546));
#16525=CARTESIAN_POINT('',(384.,28.8220324668729,15.2323346382546));
#16526=CARTESIAN_POINT('',(47.9470000000001,30.369113052182,13.));
#16527=CARTESIAN_POINT('',(47.9470000000001,28.8220324668729,15.2323346382546));
#16528=CARTESIAN_POINT('',(384.,30.369113052182,13.));
#16529=CARTESIAN_POINT('Origin',(384.,30.465859005635,16.3715599497981));
#16530=CARTESIAN_POINT('',(384.,28.4964083757143,16.7197900695531));
#16531=CARTESIAN_POINT('Origin',(384.,30.465859005635,16.3715599497981));
#16532=CARTESIAN_POINT('',(47.9470000000001,28.4964083757143,16.7197900695531));
#16533=CARTESIAN_POINT('',(384.,28.4964083757143,16.7197900695531));
#16534=CARTESIAN_POINT('Origin',(47.9470000000001,30.465859005635,16.3715599497981));
#16535=CARTESIAN_POINT('Origin',(384.,28.7029146884407,17.8877073880428));
#16536=CARTESIAN_POINT('',(384.,28.7029146884407,17.8877073880428));
#16537=CARTESIAN_POINT('',(384.,28.7029146884407,17.8877073880428));
#16538=CARTESIAN_POINT('',(47.9470000000001,28.7029146884407,17.8877073880428));
#16539=CARTESIAN_POINT('',(384.,28.7029146884407,17.8877073880428));
#16540=CARTESIAN_POINT('',(47.9470000000001,28.7029146884407,17.8877073880428));
#16541=CARTESIAN_POINT('Origin',(384.,28.2105520309605,17.9747649179816));
#16542=CARTESIAN_POINT('',(384.,28.2105520309605,18.4747649179816));
#16543=CARTESIAN_POINT('Origin',(384.,28.2105520309605,17.9747649179816));
#16544=CARTESIAN_POINT('',(47.9470000000001,28.2105520309605,18.4747649179816));
#16545=CARTESIAN_POINT('',(384.,28.2105520309605,18.4747649179816));
#16546=CARTESIAN_POINT('Origin',(47.9470000000001,28.2105520309605,17.9747649179816));
#16547=CARTESIAN_POINT('Origin',(384.,29.4028795176614,18.9747649179816));
#16548=CARTESIAN_POINT('',(384.,29.4028795176614,19.4747649179816));
#16549=CARTESIAN_POINT('Origin',(384.,29.4028795176614,18.9747649179816));
#16550=CARTESIAN_POINT('',(47.9470000000001,29.4028795176614,19.4747649179816));
#16551=CARTESIAN_POINT('Origin',(47.9470000000001,29.4028795176614,18.9747649179816));
#16552=CARTESIAN_POINT('',(384.,29.4028795176614,19.4747649179816));
#16553=CARTESIAN_POINT('Origin',(384.,25.0009567389882,18.4747649179816));
#16554=CARTESIAN_POINT('',(384.,21.7894479690395,18.4747649179816));
#16555=CARTESIAN_POINT('',(384.,25.0009567389882,18.4747649179816));
#16556=CARTESIAN_POINT('',(47.9470000000001,21.7894479690395,18.4747649179816));
#16557=CARTESIAN_POINT('',(384.,21.7894479690395,18.4747649179816));
#16558=CARTESIAN_POINT('',(47.9470000000001,24.9990432610118,18.4747649179816));
#16559=CARTESIAN_POINT('Origin',(384.,20.5188663093253,16.5456750096756));
#16560=CARTESIAN_POINT('',(384.,20.1047578248584,18.8877073880428));
#16561=CARTESIAN_POINT('',(384.,20.5188663093253,16.5456750096756));
#16562=CARTESIAN_POINT('',(384.,20.1047578248584,18.8877073880428));
#16563=CARTESIAN_POINT('',(47.9470000000001,20.1047578248584,18.8877073880428));
#16564=CARTESIAN_POINT('',(384.,20.1047578248584,18.8877073880428));
#16565=CARTESIAN_POINT('',(47.9470000000001,20.5188663093253,16.5456750096756));
#16566=CARTESIAN_POINT('',(47.9470000000001,20.1047578248584,18.8877073880428));
#16567=CARTESIAN_POINT('',(384.,20.5188663093253,16.5456750096756));
#16568=CARTESIAN_POINT('Origin',(384.,19.534140994365,16.3715599497981));
#16569=CARTESIAN_POINT('',(384.,20.356054263746,15.8019472940264));
#16570=CARTESIAN_POINT('Origin',(384.,19.534140994365,16.3715599497981));
#16571=CARTESIAN_POINT('',(47.9470000000001,20.356054263746,15.8019472940264));
#16572=CARTESIAN_POINT('Origin',(47.9470000000001,19.534140994365,16.3715599497981));
#16573=CARTESIAN_POINT('',(384.,20.356054263746,15.8019472940264));
#16574=CARTESIAN_POINT('Origin',(384.,18.4142135623731,13.));
#16575=CARTESIAN_POINT('',(384.,18.4142135623731,13.));
#16576=CARTESIAN_POINT('',(384.,20.356054263746,15.8019472940264));
#16577=CARTESIAN_POINT('',(47.9470000000001,18.4142135623731,13.));
#16578=CARTESIAN_POINT('',(47.9470000000001,20.356054263746,15.8019472940264));
#16579=CARTESIAN_POINT('',(384.,18.4142135623731,13.));
#16580=CARTESIAN_POINT('Origin',(384.,21.1779675331271,15.2323346382546));
#16581=CARTESIAN_POINT('',(384.,21.1779675331271,15.2323346382546));
#16582=CARTESIAN_POINT('',(384.,19.630886947818,13.));
#16583=CARTESIAN_POINT('',(384.,21.1779675331271,15.2323346382546));
#16584=CARTESIAN_POINT('',(47.9470000000001,19.630886947818,13.));
#16585=CARTESIAN_POINT('',(384.,19.630886947818,13.));
#16586=CARTESIAN_POINT('',(47.9470000000001,21.1779675331271,15.2323346382546));
#16587=CARTESIAN_POINT('',(47.9470000000001,21.1779675331271,15.2323346382546));
#16588=CARTESIAN_POINT('',(384.,21.1779675331271,15.2323346382546));
#16589=CARTESIAN_POINT('Origin',(384.,19.534140994365,16.3715599497981));
#16590=CARTESIAN_POINT('',(384.,21.5035916242857,16.7197900695531));
#16591=CARTESIAN_POINT('Origin',(384.,19.534140994365,16.3715599497981));
#16592=CARTESIAN_POINT('',(47.9470000000001,21.5035916242857,16.7197900695531));
#16593=CARTESIAN_POINT('Origin',(47.9470000000001,19.534140994365,16.3715599497981));
#16594=CARTESIAN_POINT('',(384.,21.5035916242857,16.7197900695531));
#16595=CARTESIAN_POINT('Origin',(384.,21.2970853115593,17.8877073880428));
#16596=CARTESIAN_POINT('',(384.,21.2970853115593,17.8877073880428));
#16597=CARTESIAN_POINT('',(384.,21.2970853115593,17.8877073880428));
#16598=CARTESIAN_POINT('',(47.9470000000001,21.2970853115593,17.8877073880428));
#16599=CARTESIAN_POINT('',(47.9470000000001,21.2970853115593,17.8877073880428));
#16600=CARTESIAN_POINT('',(384.,21.2970853115593,17.8877073880428));
#16601=CARTESIAN_POINT('Origin',(384.,21.7894479690395,17.9747649179816));
#16602=CARTESIAN_POINT('Origin',(384.,21.7894479690395,17.9747649179816));
#16603=CARTESIAN_POINT('Origin',(47.9470000000001,21.7894479690395,17.9747649179816));
#16604=CARTESIAN_POINT('Origin',(384.,20.5971204823386,19.4747649179816));
#16605=CARTESIAN_POINT('',(47.9470000000001,20.5971204823386,19.4747649179816));
#16606=CARTESIAN_POINT('',(47.9470000000001,25.0009567389882,19.4747649179816));
#16607=CARTESIAN_POINT('',(384.,20.5971204823386,19.4747649179816));
#16608=CARTESIAN_POINT('',(384.,20.5971204823386,19.4747649179816));
#16609=CARTESIAN_POINT('',(384.,25.0009567389882,19.4747649179816));
#16610=CARTESIAN_POINT('Origin',(384.,20.5971204823386,18.9747649179816));
#16611=CARTESIAN_POINT('Origin',(384.,20.5971204823386,18.9747649179816));
#16612=CARTESIAN_POINT('Origin',(47.9470000000001,20.5971204823386,18.9747649179816));
#16613=CARTESIAN_POINT('Origin',(384.,15.8284271247462,13.));
#16614=CARTESIAN_POINT('',(47.9470000000001,15.8284271247462,13.));
#16615=CARTESIAN_POINT('',(47.9470000000001,21.,13.));
#16616=CARTESIAN_POINT('',(384.,15.8284271247462,13.));
#16617=CARTESIAN_POINT('',(384.,15.8284271247462,13.));
#16618=CARTESIAN_POINT('',(384.,21.,13.));
#16619=CARTESIAN_POINT('Origin',(384.,15.8284271247462,13.));
#16620=CARTESIAN_POINT('',(384.,34.1715728752538,13.));
#16621=CARTESIAN_POINT('',(384.,21.,13.));
#16622=CARTESIAN_POINT('',(47.9470000000001,34.1715728752538,13.));
#16623=CARTESIAN_POINT('',(384.,34.1715728752538,13.));
#16624=CARTESIAN_POINT('',(47.9470000000001,21.,13.));
#16625=CARTESIAN_POINT('Origin',(384.,15.8284271247462,13.));
#16626=CARTESIAN_POINT('',(47.9470000000001,21.,13.));
#16627=CARTESIAN_POINT('',(384.,21.,13.));
#16628=CARTESIAN_POINT('Origin',(384.,34.1715728752538,14.));
#16629=CARTESIAN_POINT('',(384.,34.8786796564404,13.2928932188135));
#16630=CARTESIAN_POINT('Origin',(384.,34.1715728752538,14.));
#16631=CARTESIAN_POINT('',(47.9470000000001,34.8786796564404,13.2928932188135));
#16632=CARTESIAN_POINT('',(384.,34.8786796564404,13.2928932188135));
#16633=CARTESIAN_POINT('Origin',(47.9470000000001,34.1715728752538,14.));
#16634=CARTESIAN_POINT('Origin',(384.,37.3825273013137,15.7967408636868));
#16635=CARTESIAN_POINT('',(384.,37.3825273013137,15.7967408636868));
#16636=CARTESIAN_POINT('',(384.,34.8786796564404,13.2928932188135));
#16637=CARTESIAN_POINT('',(47.9470000000001,37.3825273013137,15.7967408636868));
#16638=CARTESIAN_POINT('',(384.,37.3825273013137,15.7967408636868));
#16639=CARTESIAN_POINT('',(47.9470000000001,34.8786796564404,13.2928932188135));
#16640=CARTESIAN_POINT('Origin',(384.,36.6754205201272,16.5038476448733));
#16641=CARTESIAN_POINT('',(384.,37.6602282731394,16.3301994672064));
#16642=CARTESIAN_POINT('Origin',(384.,36.6754205201272,16.5038476448733));
#16643=CARTESIAN_POINT('',(47.9470000000001,37.6602282731394,16.3301994672064));
#16644=CARTESIAN_POINT('',(384.,37.6602282731394,16.3301994672064));
#16645=CARTESIAN_POINT('Origin',(47.9470000000001,36.6754205201272,16.5038476448733));
#16646=CARTESIAN_POINT('Origin',(384.,38.2147000047147,19.4747649179816));
#16647=CARTESIAN_POINT('',(384.,38.2147000047147,19.4747649179816));
#16648=CARTESIAN_POINT('',(384.,37.6602282731394,16.3301994672064));
#16649=CARTESIAN_POINT('',(47.9470000000001,38.2147000047147,19.4747649179816));
#16650=CARTESIAN_POINT('',(384.,38.2147000047147,19.4747649179816));
#16651=CARTESIAN_POINT('',(47.9470000000001,37.6602282731394,16.3301994672064));
#16652=CARTESIAN_POINT('Origin',(384.,39.2301266166005,19.4747649179816));
#16653=CARTESIAN_POINT('',(384.,39.2301266166005,19.4747649179816));
#16654=CARTESIAN_POINT('',(384.,39.2301266166005,19.4747649179816));
#16655=CARTESIAN_POINT('',(47.9470000000001,39.2301266166005,19.4747649179816));
#16656=CARTESIAN_POINT('',(384.,39.2301266166005,19.4747649179816));
#16657=CARTESIAN_POINT('',(47.9470000000001,39.2301266166005,19.4747649179816));
#16658=CARTESIAN_POINT('Origin',(384.,38.6450360261516,16.1565512895395));
#16659=CARTESIAN_POINT('',(384.,38.6450360261516,16.1565512895395));
#16660=CARTESIAN_POINT('',(384.,38.6450360261516,16.1565512895395));
#16661=CARTESIAN_POINT('',(47.9470000000001,38.6450360261516,16.1565512895395));
#16662=CARTESIAN_POINT('',(384.,38.6450360261516,16.1565512895395));
#16663=CARTESIAN_POINT('',(47.9470000000001,38.6450360261516,16.1565512895395));
#16664=CARTESIAN_POINT('Origin',(384.,36.6754205201272,16.5038476448733));
#16665=CARTESIAN_POINT('',(384.,38.0896340825003,15.0896340825003));
#16666=CARTESIAN_POINT('Origin',(384.,36.6754205201272,16.5038476448733));
#16667=CARTESIAN_POINT('',(47.9470000000001,38.0896340825003,15.0896340825003));
#16668=CARTESIAN_POINT('',(384.,38.0896340825003,15.0896340825003));
#16669=CARTESIAN_POINT('Origin',(47.9470000000001,36.6754205201272,16.5038476448733));
#16670=CARTESIAN_POINT('Origin',(384.,35.5857864376269,12.5857864376269));
#16671=CARTESIAN_POINT('',(384.,35.5857864376269,12.5857864376269));
#16672=CARTESIAN_POINT('',(384.,35.5857864376269,12.5857864376269));
#16673=CARTESIAN_POINT('',(47.9470000000001,35.5857864376269,12.5857864376269));
#16674=CARTESIAN_POINT('',(384.,35.5857864376269,12.5857864376269));
#16675=CARTESIAN_POINT('',(47.9470000000001,35.5857864376269,12.5857864376269));
#16676=CARTESIAN_POINT('Origin',(384.,34.1715728752538,14.));
#16677=CARTESIAN_POINT('',(384.,34.1715728752538,12.));
#16678=CARTESIAN_POINT('Origin',(384.,34.1715728752538,14.));
#16679=CARTESIAN_POINT('',(47.9470000000001,34.1715728752538,12.));
#16680=CARTESIAN_POINT('',(384.,34.1715728752538,12.));
#16681=CARTESIAN_POINT('Origin',(47.9470000000001,34.1715728752538,14.));
#16682=CARTESIAN_POINT('Origin',(384.,25.,12.));
#16683=CARTESIAN_POINT('',(384.,15.8284271247462,12.));
#16684=CARTESIAN_POINT('',(384.,25.,12.));
#16685=CARTESIAN_POINT('',(47.9470000000001,15.8284271247462,12.));
#16686=CARTESIAN_POINT('',(384.,15.8284271247462,12.));
#16687=CARTESIAN_POINT('',(47.9470000000001,25.,12.));
#16688=CARTESIAN_POINT('Origin',(384.,15.8284271247462,14.));
#16689=CARTESIAN_POINT('',(384.,15.1213203435596,13.2928932188135));
#16690=CARTESIAN_POINT('Origin',(384.,15.8284271247462,14.));
#16691=CARTESIAN_POINT('',(47.9470000000001,15.1213203435596,13.2928932188135));
#16692=CARTESIAN_POINT('Origin',(47.9470000000001,15.8284271247462,14.));
#16693=CARTESIAN_POINT('',(384.,15.1213203435596,13.2928932188135));
#16694=CARTESIAN_POINT('Origin',(384.,12.6174726986863,15.7967408636868));
#16695=CARTESIAN_POINT('',(384.,12.6174726986863,15.7967408636868));
#16696=CARTESIAN_POINT('',(384.,15.1213203435596,13.2928932188135));
#16697=CARTESIAN_POINT('',(47.9470000000001,12.6174726986863,15.7967408636868));
#16698=CARTESIAN_POINT('',(47.9470000000001,15.1213203435596,13.2928932188135));
#16699=CARTESIAN_POINT('',(384.,12.6174726986863,15.7967408636868));
#16700=CARTESIAN_POINT('Origin',(384.,13.3245794798728,16.5038476448733));
#16701=CARTESIAN_POINT('',(384.,12.3397717268606,16.3301994672064));
#16702=CARTESIAN_POINT('Origin',(384.,13.3245794798728,16.5038476448733));
#16703=CARTESIAN_POINT('',(47.9470000000001,12.3397717268606,16.3301994672064));
#16704=CARTESIAN_POINT('Origin',(47.9470000000001,13.3245794798728,16.5038476448733));
#16705=CARTESIAN_POINT('',(384.,12.3397717268606,16.3301994672064));
#16706=CARTESIAN_POINT('Origin',(384.,11.7852999952853,19.4747649179816));
#16707=CARTESIAN_POINT('',(384.,11.7852999952853,19.4747649179816));
#16708=CARTESIAN_POINT('',(384.,12.3397717268606,16.3301994672064));
#16709=CARTESIAN_POINT('',(47.9470000000001,11.7852999952853,19.4747649179816));
#16710=CARTESIAN_POINT('',(47.9470000000001,12.3397717268606,16.3301994672064));
#16711=CARTESIAN_POINT('',(384.,11.7852999952853,19.4747649179816));
#16712=CARTESIAN_POINT('Origin',(384.,10.7698733833995,19.4747649179816));
#16713=CARTESIAN_POINT('',(384.,10.7698733833995,19.4747649179816));
#16714=CARTESIAN_POINT('',(384.,10.7698733833995,19.4747649179816));
#16715=CARTESIAN_POINT('',(47.9470000000001,10.7698733833995,19.4747649179816));
#16716=CARTESIAN_POINT('',(47.9470000000001,10.7698733833995,19.4747649179816));
#16717=CARTESIAN_POINT('',(384.,10.7698733833995,19.4747649179816));
#16718=CARTESIAN_POINT('Origin',(384.,11.3549639738484,16.1565512895395));
#16719=CARTESIAN_POINT('',(384.,11.3549639738484,16.1565512895395));
#16720=CARTESIAN_POINT('',(384.,11.3549639738484,16.1565512895395));
#16721=CARTESIAN_POINT('',(47.9470000000001,11.3549639738484,16.1565512895395));
#16722=CARTESIAN_POINT('',(47.9470000000001,11.3549639738484,16.1565512895395));
#16723=CARTESIAN_POINT('',(384.,11.3549639738484,16.1565512895395));
#16724=CARTESIAN_POINT('Origin',(384.,13.3245794798728,16.5038476448733));
#16725=CARTESIAN_POINT('',(384.,11.9103659174997,15.0896340825003));
#16726=CARTESIAN_POINT('Origin',(384.,13.3245794798728,16.5038476448733));
#16727=CARTESIAN_POINT('',(47.9470000000001,11.9103659174997,15.0896340825003));
#16728=CARTESIAN_POINT('Origin',(47.9470000000001,13.3245794798728,16.5038476448733));
#16729=CARTESIAN_POINT('',(384.,11.9103659174997,15.0896340825003));
#16730=CARTESIAN_POINT('Origin',(384.,14.4142135623731,12.5857864376269));
#16731=CARTESIAN_POINT('',(384.,14.4142135623731,12.5857864376269));
#16732=CARTESIAN_POINT('',(384.,14.4142135623731,12.5857864376269));
#16733=CARTESIAN_POINT('',(47.9470000000001,14.4142135623731,12.5857864376269));
#16734=CARTESIAN_POINT('',(47.9470000000001,14.4142135623731,12.5857864376269));
#16735=CARTESIAN_POINT('',(384.,14.4142135623731,12.5857864376269));
#16736=CARTESIAN_POINT('Origin',(384.,15.8284271247462,14.));
#16737=CARTESIAN_POINT('Origin',(384.,15.8284271247462,14.));
#16738=CARTESIAN_POINT('Origin',(47.9470000000001,15.8284271247462,14.));
#16739=CARTESIAN_POINT('Origin',(384.,17.8849366916998,15.7373824589908));
#16740=CARTESIAN_POINT('Origin',(47.9470000000001,17.8849366916998,15.7373824589908));
#16741=CARTESIAN_POINT('',(0.,0.,0.));
#16742=CARTESIAN_POINT('Origin',(351.940084821141,11.70240347792,12.));
#16743=CARTESIAN_POINT('',(354.440084821141,11.70240347792,12.));
#16744=CARTESIAN_POINT('Origin',(351.940084821141,11.70240347792,12.));
#16745=CARTESIAN_POINT('',(354.440084821141,11.70240347792,10.));
#16746=CARTESIAN_POINT('',(354.440084821141,11.70240347792,12.));
#16747=CARTESIAN_POINT('Origin',(351.940084821141,11.70240347792,10.));
#16748=CARTESIAN_POINT('Origin',(378.352975097007,11.70240347792,12.));
#16749=CARTESIAN_POINT('',(380.852975097007,11.70240347792,12.));
#16750=CARTESIAN_POINT('Origin',(378.352975097007,11.70240347792,12.));
#16751=CARTESIAN_POINT('',(380.852975097007,11.70240347792,10.));
#16752=CARTESIAN_POINT('',(380.852975097007,11.70240347792,12.));
#16753=CARTESIAN_POINT('Origin',(378.352975097007,11.70240347792,10.));
#16754=CARTESIAN_POINT('Origin',(378.352975097007,38.29759652208,12.));
#16755=CARTESIAN_POINT('',(380.852975097007,38.29759652208,12.));
#16756=CARTESIAN_POINT('Origin',(378.352975097007,38.29759652208,12.));
#16757=CARTESIAN_POINT('',(380.852975097007,38.29759652208,10.));
#16758=CARTESIAN_POINT('',(380.852975097007,38.29759652208,12.));
#16759=CARTESIAN_POINT('Origin',(378.352975097007,38.29759652208,10.));
#16760=CARTESIAN_POINT('Origin',(351.940084821141,38.29759652208,12.));
#16761=CARTESIAN_POINT('',(354.440084821141,38.29759652208,12.));
#16762=CARTESIAN_POINT('Origin',(351.940084821141,38.29759652208,12.));
#16763=CARTESIAN_POINT('',(354.440084821141,38.29759652208,10.));
#16764=CARTESIAN_POINT('',(354.440084821141,38.29759652208,12.));
#16765=CARTESIAN_POINT('Origin',(351.940084821141,38.29759652208,10.));
#16766=CARTESIAN_POINT('Origin',(365.146529959074,25.,12.));
#16767=CARTESIAN_POINT('',(375.146529959074,25.,12.));
#16768=CARTESIAN_POINT('Origin',(365.146529959074,25.,12.));
#16769=CARTESIAN_POINT('',(375.146529959074,25.,10.));
#16770=CARTESIAN_POINT('',(375.146529959074,25.,12.));
#16771=CARTESIAN_POINT('Origin',(365.146529959074,25.,10.));
#16772=CARTESIAN_POINT('Origin',(363.646529959074,39.8065050734778,12.));
#16773=CARTESIAN_POINT('',(363.646529959074,44.7051656728289,10.));
#16774=CARTESIAN_POINT('',(363.646529959074,39.8065050734778,10.));
#16775=CARTESIAN_POINT('',(363.646529959074,19.9032525367389,10.));
#16776=CARTESIAN_POINT('',(363.646529959074,44.7051656728289,12.));
#16777=CARTESIAN_POINT('',(363.646529959074,44.7051656728289,12.));
#16778=CARTESIAN_POINT('',(363.646529959074,39.8065050734778,12.));
#16779=CARTESIAN_POINT('',(363.646529959074,19.9032525367389,12.));
#16780=CARTESIAN_POINT('',(363.646529959074,39.8065050734778,12.));
#16781=CARTESIAN_POINT('Origin',(365.146529959074,39.8065050734778,12.));
#16782=CARTESIAN_POINT('',(366.646529959074,39.8065050734778,10.));
#16783=CARTESIAN_POINT('Origin',(365.146529959074,39.8065050734778,10.));
#16784=CARTESIAN_POINT('',(366.646529959074,39.8065050734778,12.));
#16785=CARTESIAN_POINT('Origin',(365.146529959074,39.8065050734778,12.));
#16786=CARTESIAN_POINT('',(366.646529959074,39.8065050734778,12.));
#16787=CARTESIAN_POINT('Origin',(366.646529959074,44.7051656728289,12.));
#16788=CARTESIAN_POINT('',(366.646529959074,44.7051656728289,10.));
#16789=CARTESIAN_POINT('',(366.646529959074,22.3525828364145,10.));
#16790=CARTESIAN_POINT('',(366.646529959074,44.7051656728289,12.));
#16791=CARTESIAN_POINT('',(366.646529959074,22.3525828364145,12.));
#16792=CARTESIAN_POINT('',(366.646529959074,44.7051656728289,12.));
#16793=CARTESIAN_POINT('Origin',(365.146529959074,44.7051656728289,12.));
#16794=CARTESIAN_POINT('Origin',(365.146529959074,44.7051656728289,10.));
#16795=CARTESIAN_POINT('Origin',(365.146529959074,44.7051656728289,12.));
#16796=CARTESIAN_POINT('Origin',(363.646529959074,5.29483432717106,12.));
#16797=CARTESIAN_POINT('',(363.646529959074,10.1934949265222,10.));
#16798=CARTESIAN_POINT('',(363.646529959074,5.29483432717106,10.));
#16799=CARTESIAN_POINT('',(363.646529959074,2.64741716358553,10.));
#16800=CARTESIAN_POINT('',(363.646529959074,10.1934949265222,12.));
#16801=CARTESIAN_POINT('',(363.646529959074,10.1934949265222,12.));
#16802=CARTESIAN_POINT('',(363.646529959074,5.29483432717106,12.));
#16803=CARTESIAN_POINT('',(363.646529959074,2.64741716358553,12.));
#16804=CARTESIAN_POINT('',(363.646529959074,5.29483432717106,12.));
#16805=CARTESIAN_POINT('Origin',(365.146529959074,5.29483432717106,12.));
#16806=CARTESIAN_POINT('',(366.646529959074,5.29483432717106,10.));
#16807=CARTESIAN_POINT('Origin',(365.146529959074,5.29483432717106,10.));
#16808=CARTESIAN_POINT('',(366.646529959074,5.29483432717106,12.));
#16809=CARTESIAN_POINT('Origin',(365.146529959074,5.29483432717106,12.));
#16810=CARTESIAN_POINT('',(366.646529959074,5.29483432717106,12.));
#16811=CARTESIAN_POINT('Origin',(366.646529959074,10.1934949265222,12.));
#16812=CARTESIAN_POINT('',(366.646529959074,10.1934949265222,10.));
#16813=CARTESIAN_POINT('',(366.646529959074,5.09674746326108,10.));
#16814=CARTESIAN_POINT('',(366.646529959074,10.1934949265222,12.));
#16815=CARTESIAN_POINT('',(366.646529959074,5.09674746326108,12.));
#16816=CARTESIAN_POINT('',(366.646529959074,10.1934949265222,12.));
#16817=CARTESIAN_POINT('Origin',(365.146529959074,10.1934949265222,12.));
#16818=CARTESIAN_POINT('Origin',(365.146529959074,10.1934949265222,10.));
#16819=CARTESIAN_POINT('Origin',(365.146529959074,10.1934949265222,12.));
#16820=CARTESIAN_POINT('Origin',(313.495640376696,11.70240347792,12.));
#16821=CARTESIAN_POINT('',(315.995640376696,11.70240347792,12.));
#16822=CARTESIAN_POINT('Origin',(313.495640376696,11.70240347792,12.));
#16823=CARTESIAN_POINT('',(315.995640376696,11.70240347792,10.));
#16824=CARTESIAN_POINT('',(315.995640376696,11.70240347792,12.));
#16825=CARTESIAN_POINT('Origin',(313.495640376696,11.70240347792,10.));
#16826=CARTESIAN_POINT('Origin',(339.908530652563,11.70240347792,12.));
#16827=CARTESIAN_POINT('',(342.408530652563,11.70240347792,12.));
#16828=CARTESIAN_POINT('Origin',(339.908530652563,11.70240347792,12.));
#16829=CARTESIAN_POINT('',(342.408530652563,11.70240347792,10.));
#16830=CARTESIAN_POINT('',(342.408530652563,11.70240347792,12.));
#16831=CARTESIAN_POINT('Origin',(339.908530652563,11.70240347792,10.));
#16832=CARTESIAN_POINT('Origin',(339.908530652563,38.29759652208,12.));
#16833=CARTESIAN_POINT('',(342.408530652563,38.29759652208,12.));
#16834=CARTESIAN_POINT('Origin',(339.908530652563,38.29759652208,12.));
#16835=CARTESIAN_POINT('',(342.408530652563,38.29759652208,10.));
#16836=CARTESIAN_POINT('',(342.408530652563,38.29759652208,12.));
#16837=CARTESIAN_POINT('Origin',(339.908530652563,38.29759652208,10.));
#16838=CARTESIAN_POINT('Origin',(313.495640376696,38.29759652208,12.));
#16839=CARTESIAN_POINT('',(315.995640376696,38.29759652208,12.));
#16840=CARTESIAN_POINT('Origin',(313.495640376696,38.29759652208,12.));
#16841=CARTESIAN_POINT('',(315.995640376696,38.29759652208,10.));
#16842=CARTESIAN_POINT('',(315.995640376696,38.29759652208,12.));
#16843=CARTESIAN_POINT('Origin',(313.495640376696,38.29759652208,10.));
#16844=CARTESIAN_POINT('Origin',(326.70208551463,25.,12.));
#16845=CARTESIAN_POINT('',(336.70208551463,25.,12.));
#16846=CARTESIAN_POINT('Origin',(326.70208551463,25.,12.));
#16847=CARTESIAN_POINT('',(336.70208551463,25.,10.));
#16848=CARTESIAN_POINT('',(336.70208551463,25.,12.));
#16849=CARTESIAN_POINT('Origin',(326.70208551463,25.,10.));
#16850=CARTESIAN_POINT('Origin',(325.20208551463,39.8065050734778,12.));
#16851=CARTESIAN_POINT('',(325.20208551463,44.7051656728289,10.));
#16852=CARTESIAN_POINT('',(325.20208551463,39.8065050734778,10.));
#16853=CARTESIAN_POINT('',(325.20208551463,19.9032525367389,10.));
#16854=CARTESIAN_POINT('',(325.20208551463,44.7051656728289,12.));
#16855=CARTESIAN_POINT('',(325.20208551463,44.7051656728289,12.));
#16856=CARTESIAN_POINT('',(325.20208551463,39.8065050734778,12.));
#16857=CARTESIAN_POINT('',(325.20208551463,19.9032525367389,12.));
#16858=CARTESIAN_POINT('',(325.20208551463,39.8065050734778,12.));
#16859=CARTESIAN_POINT('Origin',(326.70208551463,39.8065050734778,12.));
#16860=CARTESIAN_POINT('',(328.20208551463,39.8065050734778,10.));
#16861=CARTESIAN_POINT('Origin',(326.70208551463,39.8065050734778,10.));
#16862=CARTESIAN_POINT('',(328.20208551463,39.8065050734778,12.));
#16863=CARTESIAN_POINT('Origin',(326.70208551463,39.8065050734778,12.));
#16864=CARTESIAN_POINT('',(328.20208551463,39.8065050734778,12.));
#16865=CARTESIAN_POINT('Origin',(328.20208551463,44.7051656728289,12.));
#16866=CARTESIAN_POINT('',(328.20208551463,44.7051656728289,10.));
#16867=CARTESIAN_POINT('',(328.20208551463,22.3525828364145,10.));
#16868=CARTESIAN_POINT('',(328.20208551463,44.7051656728289,12.));
#16869=CARTESIAN_POINT('',(328.20208551463,22.3525828364145,12.));
#16870=CARTESIAN_POINT('',(328.20208551463,44.7051656728289,12.));
#16871=CARTESIAN_POINT('Origin',(326.70208551463,44.7051656728289,12.));
#16872=CARTESIAN_POINT('Origin',(326.70208551463,44.7051656728289,10.));
#16873=CARTESIAN_POINT('Origin',(326.70208551463,44.7051656728289,12.));
#16874=CARTESIAN_POINT('Origin',(325.20208551463,5.29483432717106,12.));
#16875=CARTESIAN_POINT('',(325.20208551463,10.1934949265222,10.));
#16876=CARTESIAN_POINT('',(325.20208551463,5.29483432717106,10.));
#16877=CARTESIAN_POINT('',(325.20208551463,2.64741716358553,10.));
#16878=CARTESIAN_POINT('',(325.20208551463,10.1934949265222,12.));
#16879=CARTESIAN_POINT('',(325.20208551463,10.1934949265222,12.));
#16880=CARTESIAN_POINT('',(325.20208551463,5.29483432717106,12.));
#16881=CARTESIAN_POINT('',(325.20208551463,2.64741716358553,12.));
#16882=CARTESIAN_POINT('',(325.20208551463,5.29483432717106,12.));
#16883=CARTESIAN_POINT('Origin',(326.70208551463,5.29483432717106,12.));
#16884=CARTESIAN_POINT('',(328.20208551463,5.29483432717106,10.));
#16885=CARTESIAN_POINT('Origin',(326.70208551463,5.29483432717106,10.));
#16886=CARTESIAN_POINT('',(328.20208551463,5.29483432717106,12.));
#16887=CARTESIAN_POINT('Origin',(326.70208551463,5.29483432717106,12.));
#16888=CARTESIAN_POINT('',(328.20208551463,5.29483432717106,12.));
#16889=CARTESIAN_POINT('Origin',(328.20208551463,10.1934949265222,12.));
#16890=CARTESIAN_POINT('',(328.20208551463,10.1934949265222,10.));
#16891=CARTESIAN_POINT('',(328.20208551463,5.09674746326108,10.));
#16892=CARTESIAN_POINT('',(328.20208551463,10.1934949265222,12.));
#16893=CARTESIAN_POINT('',(328.20208551463,5.09674746326108,12.));
#16894=CARTESIAN_POINT('',(328.20208551463,10.1934949265222,12.));
#16895=CARTESIAN_POINT('Origin',(326.70208551463,10.1934949265222,12.));
#16896=CARTESIAN_POINT('Origin',(326.70208551463,10.1934949265222,10.));
#16897=CARTESIAN_POINT('Origin',(326.70208551463,10.1934949265222,12.));
#16898=CARTESIAN_POINT('Origin',(275.051195932252,11.70240347792,12.));
#16899=CARTESIAN_POINT('',(277.551195932252,11.70240347792,12.));
#16900=CARTESIAN_POINT('Origin',(275.051195932252,11.70240347792,12.));
#16901=CARTESIAN_POINT('',(277.551195932252,11.70240347792,10.));
#16902=CARTESIAN_POINT('',(277.551195932252,11.70240347792,12.));
#16903=CARTESIAN_POINT('Origin',(275.051195932252,11.70240347792,10.));
#16904=CARTESIAN_POINT('Origin',(301.464086208118,11.70240347792,12.));
#16905=CARTESIAN_POINT('',(303.964086208118,11.70240347792,12.));
#16906=CARTESIAN_POINT('Origin',(301.464086208118,11.70240347792,12.));
#16907=CARTESIAN_POINT('',(303.964086208118,11.70240347792,10.));
#16908=CARTESIAN_POINT('',(303.964086208118,11.70240347792,12.));
#16909=CARTESIAN_POINT('Origin',(301.464086208118,11.70240347792,10.));
#16910=CARTESIAN_POINT('Origin',(301.464086208118,38.29759652208,12.));
#16911=CARTESIAN_POINT('',(303.964086208118,38.29759652208,12.));
#16912=CARTESIAN_POINT('Origin',(301.464086208118,38.29759652208,12.));
#16913=CARTESIAN_POINT('',(303.964086208118,38.29759652208,10.));
#16914=CARTESIAN_POINT('',(303.964086208118,38.29759652208,12.));
#16915=CARTESIAN_POINT('Origin',(301.464086208118,38.29759652208,10.));
#16916=CARTESIAN_POINT('Origin',(275.051195932252,38.29759652208,12.));
#16917=CARTESIAN_POINT('',(277.551195932252,38.29759652208,12.));
#16918=CARTESIAN_POINT('Origin',(275.051195932252,38.29759652208,12.));
#16919=CARTESIAN_POINT('',(277.551195932252,38.29759652208,10.));
#16920=CARTESIAN_POINT('',(277.551195932252,38.29759652208,12.));
#16921=CARTESIAN_POINT('Origin',(275.051195932252,38.29759652208,10.));
#16922=CARTESIAN_POINT('Origin',(288.257641070185,25.,12.));
#16923=CARTESIAN_POINT('',(298.257641070185,25.,12.));
#16924=CARTESIAN_POINT('Origin',(288.257641070185,25.,12.));
#16925=CARTESIAN_POINT('',(298.257641070185,25.,10.));
#16926=CARTESIAN_POINT('',(298.257641070185,25.,12.));
#16927=CARTESIAN_POINT('Origin',(288.257641070185,25.,10.));
#16928=CARTESIAN_POINT('Origin',(286.757641070185,39.8065050734778,12.));
#16929=CARTESIAN_POINT('',(286.757641070185,44.7051656728289,10.));
#16930=CARTESIAN_POINT('',(286.757641070185,39.8065050734778,10.));
#16931=CARTESIAN_POINT('',(286.757641070185,19.9032525367389,10.));
#16932=CARTESIAN_POINT('',(286.757641070185,44.7051656728289,12.));
#16933=CARTESIAN_POINT('',(286.757641070185,44.7051656728289,12.));
#16934=CARTESIAN_POINT('',(286.757641070185,39.8065050734778,12.));
#16935=CARTESIAN_POINT('',(286.757641070185,19.9032525367389,12.));
#16936=CARTESIAN_POINT('',(286.757641070185,39.8065050734778,12.));
#16937=CARTESIAN_POINT('Origin',(288.257641070185,39.8065050734778,12.));
#16938=CARTESIAN_POINT('',(289.757641070185,39.8065050734778,10.));
#16939=CARTESIAN_POINT('Origin',(288.257641070185,39.8065050734778,10.));
#16940=CARTESIAN_POINT('',(289.757641070185,39.8065050734778,12.));
#16941=CARTESIAN_POINT('Origin',(288.257641070185,39.8065050734778,12.));
#16942=CARTESIAN_POINT('',(289.757641070185,39.8065050734778,12.));
#16943=CARTESIAN_POINT('Origin',(289.757641070185,44.7051656728289,12.));
#16944=CARTESIAN_POINT('',(289.757641070185,44.7051656728289,10.));
#16945=CARTESIAN_POINT('',(289.757641070185,22.3525828364145,10.));
#16946=CARTESIAN_POINT('',(289.757641070185,44.7051656728289,12.));
#16947=CARTESIAN_POINT('',(289.757641070185,22.3525828364145,12.));
#16948=CARTESIAN_POINT('',(289.757641070185,44.7051656728289,12.));
#16949=CARTESIAN_POINT('Origin',(288.257641070185,44.7051656728289,12.));
#16950=CARTESIAN_POINT('Origin',(288.257641070185,44.7051656728289,10.));
#16951=CARTESIAN_POINT('Origin',(288.257641070185,44.7051656728289,12.));
#16952=CARTESIAN_POINT('Origin',(286.757641070185,5.29483432717106,12.));
#16953=CARTESIAN_POINT('',(286.757641070185,10.1934949265222,10.));
#16954=CARTESIAN_POINT('',(286.757641070185,5.29483432717106,10.));
#16955=CARTESIAN_POINT('',(286.757641070185,2.64741716358553,10.));
#16956=CARTESIAN_POINT('',(286.757641070185,10.1934949265222,12.));
#16957=CARTESIAN_POINT('',(286.757641070185,10.1934949265222,12.));
#16958=CARTESIAN_POINT('',(286.757641070185,5.29483432717106,12.));
#16959=CARTESIAN_POINT('',(286.757641070185,2.64741716358553,12.));
#16960=CARTESIAN_POINT('',(286.757641070185,5.29483432717106,12.));
#16961=CARTESIAN_POINT('Origin',(288.257641070185,5.29483432717106,12.));
#16962=CARTESIAN_POINT('',(289.757641070185,5.29483432717106,10.));
#16963=CARTESIAN_POINT('Origin',(288.257641070185,5.29483432717106,10.));
#16964=CARTESIAN_POINT('',(289.757641070185,5.29483432717106,12.));
#16965=CARTESIAN_POINT('Origin',(288.257641070185,5.29483432717106,12.));
#16966=CARTESIAN_POINT('',(289.757641070185,5.29483432717106,12.));
#16967=CARTESIAN_POINT('Origin',(289.757641070185,10.1934949265222,12.));
#16968=CARTESIAN_POINT('',(289.757641070185,10.1934949265222,10.));
#16969=CARTESIAN_POINT('',(289.757641070185,5.09674746326108,10.));
#16970=CARTESIAN_POINT('',(289.757641070185,10.1934949265222,12.));
#16971=CARTESIAN_POINT('',(289.757641070185,5.09674746326108,12.));
#16972=CARTESIAN_POINT('',(289.757641070185,10.1934949265222,12.));
#16973=CARTESIAN_POINT('Origin',(288.257641070185,10.1934949265222,12.));
#16974=CARTESIAN_POINT('Origin',(288.257641070185,10.1934949265222,10.));
#16975=CARTESIAN_POINT('Origin',(288.257641070185,10.1934949265222,12.));
#16976=CARTESIAN_POINT('Origin',(236.606751487807,11.70240347792,12.));
#16977=CARTESIAN_POINT('',(239.106751487807,11.70240347792,12.));
#16978=CARTESIAN_POINT('Origin',(236.606751487807,11.70240347792,12.));
#16979=CARTESIAN_POINT('',(239.106751487807,11.70240347792,10.));
#16980=CARTESIAN_POINT('',(239.106751487807,11.70240347792,12.));
#16981=CARTESIAN_POINT('Origin',(236.606751487807,11.70240347792,10.));
#16982=CARTESIAN_POINT('Origin',(263.019641763674,11.70240347792,12.));
#16983=CARTESIAN_POINT('',(265.519641763674,11.70240347792,12.));
#16984=CARTESIAN_POINT('Origin',(263.019641763674,11.70240347792,12.));
#16985=CARTESIAN_POINT('',(265.519641763674,11.70240347792,10.));
#16986=CARTESIAN_POINT('',(265.519641763674,11.70240347792,12.));
#16987=CARTESIAN_POINT('Origin',(263.019641763674,11.70240347792,10.));
#16988=CARTESIAN_POINT('Origin',(263.019641763674,38.29759652208,12.));
#16989=CARTESIAN_POINT('',(265.519641763674,38.29759652208,12.));
#16990=CARTESIAN_POINT('Origin',(263.019641763674,38.29759652208,12.));
#16991=CARTESIAN_POINT('',(265.519641763674,38.29759652208,10.));
#16992=CARTESIAN_POINT('',(265.519641763674,38.29759652208,12.));
#16993=CARTESIAN_POINT('Origin',(263.019641763674,38.29759652208,10.));
#16994=CARTESIAN_POINT('Origin',(236.606751487807,38.29759652208,12.));
#16995=CARTESIAN_POINT('',(239.106751487807,38.29759652208,12.));
#16996=CARTESIAN_POINT('Origin',(236.606751487807,38.29759652208,12.));
#16997=CARTESIAN_POINT('',(239.106751487807,38.29759652208,10.));
#16998=CARTESIAN_POINT('',(239.106751487807,38.29759652208,12.));
#16999=CARTESIAN_POINT('Origin',(236.606751487807,38.29759652208,10.));
#17000=CARTESIAN_POINT('Origin',(249.813196625741,25.,12.));
#17001=CARTESIAN_POINT('',(259.813196625741,25.,12.));
#17002=CARTESIAN_POINT('Origin',(249.813196625741,25.,12.));
#17003=CARTESIAN_POINT('',(259.813196625741,25.,10.));
#17004=CARTESIAN_POINT('',(259.813196625741,25.,12.));
#17005=CARTESIAN_POINT('Origin',(249.813196625741,25.,10.));
#17006=CARTESIAN_POINT('Origin',(248.313196625741,39.8065050734778,12.));
#17007=CARTESIAN_POINT('',(248.313196625741,44.7051656728289,10.));
#17008=CARTESIAN_POINT('',(248.313196625741,39.8065050734778,10.));
#17009=CARTESIAN_POINT('',(248.313196625741,19.9032525367389,10.));
#17010=CARTESIAN_POINT('',(248.313196625741,44.7051656728289,12.));
#17011=CARTESIAN_POINT('',(248.313196625741,44.7051656728289,12.));
#17012=CARTESIAN_POINT('',(248.313196625741,39.8065050734778,12.));
#17013=CARTESIAN_POINT('',(248.313196625741,19.9032525367389,12.));
#17014=CARTESIAN_POINT('',(248.313196625741,39.8065050734778,12.));
#17015=CARTESIAN_POINT('Origin',(249.813196625741,39.8065050734778,12.));
#17016=CARTESIAN_POINT('',(251.313196625741,39.8065050734778,10.));
#17017=CARTESIAN_POINT('Origin',(249.813196625741,39.8065050734778,10.));
#17018=CARTESIAN_POINT('',(251.313196625741,39.8065050734778,12.));
#17019=CARTESIAN_POINT('Origin',(249.813196625741,39.8065050734778,12.));
#17020=CARTESIAN_POINT('',(251.313196625741,39.8065050734778,12.));
#17021=CARTESIAN_POINT('Origin',(251.313196625741,44.7051656728289,12.));
#17022=CARTESIAN_POINT('',(251.313196625741,44.7051656728289,10.));
#17023=CARTESIAN_POINT('',(251.313196625741,22.3525828364145,10.));
#17024=CARTESIAN_POINT('',(251.313196625741,44.7051656728289,12.));
#17025=CARTESIAN_POINT('',(251.313196625741,22.3525828364145,12.));
#17026=CARTESIAN_POINT('',(251.313196625741,44.7051656728289,12.));
#17027=CARTESIAN_POINT('Origin',(249.813196625741,44.7051656728289,12.));
#17028=CARTESIAN_POINT('Origin',(249.813196625741,44.7051656728289,10.));
#17029=CARTESIAN_POINT('Origin',(249.813196625741,44.7051656728289,12.));
#17030=CARTESIAN_POINT('Origin',(248.313196625741,5.29483432717106,12.));
#17031=CARTESIAN_POINT('',(248.313196625741,10.1934949265222,10.));
#17032=CARTESIAN_POINT('',(248.313196625741,5.29483432717106,10.));
#17033=CARTESIAN_POINT('',(248.313196625741,2.64741716358553,10.));
#17034=CARTESIAN_POINT('',(248.313196625741,10.1934949265222,12.));
#17035=CARTESIAN_POINT('',(248.313196625741,10.1934949265222,12.));
#17036=CARTESIAN_POINT('',(248.313196625741,5.29483432717106,12.));
#17037=CARTESIAN_POINT('',(248.313196625741,2.64741716358553,12.));
#17038=CARTESIAN_POINT('',(248.313196625741,5.29483432717106,12.));
#17039=CARTESIAN_POINT('Origin',(249.813196625741,5.29483432717106,12.));
#17040=CARTESIAN_POINT('',(251.313196625741,5.29483432717106,10.));
#17041=CARTESIAN_POINT('Origin',(249.813196625741,5.29483432717106,10.));
#17042=CARTESIAN_POINT('',(251.313196625741,5.29483432717106,12.));
#17043=CARTESIAN_POINT('Origin',(249.813196625741,5.29483432717106,12.));
#17044=CARTESIAN_POINT('',(251.313196625741,5.29483432717106,12.));
#17045=CARTESIAN_POINT('Origin',(251.313196625741,10.1934949265222,12.));
#17046=CARTESIAN_POINT('',(251.313196625741,10.1934949265222,10.));
#17047=CARTESIAN_POINT('',(251.313196625741,5.09674746326108,10.));
#17048=CARTESIAN_POINT('',(251.313196625741,10.1934949265222,12.));
#17049=CARTESIAN_POINT('',(251.313196625741,5.09674746326108,12.));
#17050=CARTESIAN_POINT('',(251.313196625741,10.1934949265222,12.));
#17051=CARTESIAN_POINT('Origin',(249.813196625741,10.1934949265222,12.));
#17052=CARTESIAN_POINT('Origin',(249.813196625741,10.1934949265222,10.));
#17053=CARTESIAN_POINT('Origin',(249.813196625741,10.1934949265222,12.));
#17054=CARTESIAN_POINT('Origin',(198.162307043363,11.70240347792,12.));
#17055=CARTESIAN_POINT('',(200.662307043363,11.70240347792,12.));
#17056=CARTESIAN_POINT('Origin',(198.162307043363,11.70240347792,12.));
#17057=CARTESIAN_POINT('',(200.662307043363,11.70240347792,10.));
#17058=CARTESIAN_POINT('',(200.662307043363,11.70240347792,12.));
#17059=CARTESIAN_POINT('Origin',(198.162307043363,11.70240347792,10.));
#17060=CARTESIAN_POINT('Origin',(224.575197319229,11.70240347792,12.));
#17061=CARTESIAN_POINT('',(227.075197319229,11.70240347792,12.));
#17062=CARTESIAN_POINT('Origin',(224.575197319229,11.70240347792,12.));
#17063=CARTESIAN_POINT('',(227.075197319229,11.70240347792,10.));
#17064=CARTESIAN_POINT('',(227.075197319229,11.70240347792,12.));
#17065=CARTESIAN_POINT('Origin',(224.575197319229,11.70240347792,10.));
#17066=CARTESIAN_POINT('Origin',(224.575197319229,38.29759652208,12.));
#17067=CARTESIAN_POINT('',(227.075197319229,38.29759652208,12.));
#17068=CARTESIAN_POINT('Origin',(224.575197319229,38.29759652208,12.));
#17069=CARTESIAN_POINT('',(227.075197319229,38.29759652208,10.));
#17070=CARTESIAN_POINT('',(227.075197319229,38.29759652208,12.));
#17071=CARTESIAN_POINT('Origin',(224.575197319229,38.29759652208,10.));
#17072=CARTESIAN_POINT('Origin',(198.162307043363,38.29759652208,12.));
#17073=CARTESIAN_POINT('',(200.662307043363,38.29759652208,12.));
#17074=CARTESIAN_POINT('Origin',(198.162307043363,38.29759652208,12.));
#17075=CARTESIAN_POINT('',(200.662307043363,38.29759652208,10.));
#17076=CARTESIAN_POINT('',(200.662307043363,38.29759652208,12.));
#17077=CARTESIAN_POINT('Origin',(198.162307043363,38.29759652208,10.));
#17078=CARTESIAN_POINT('Origin',(211.368752181296,25.,12.));
#17079=CARTESIAN_POINT('',(221.368752181296,25.,12.));
#17080=CARTESIAN_POINT('Origin',(211.368752181296,25.,12.));
#17081=CARTESIAN_POINT('',(221.368752181296,25.,10.));
#17082=CARTESIAN_POINT('',(221.368752181296,25.,12.));
#17083=CARTESIAN_POINT('Origin',(211.368752181296,25.,10.));
#17084=CARTESIAN_POINT('Origin',(209.868752181296,39.8065050734778,12.));
#17085=CARTESIAN_POINT('',(209.868752181296,44.7051656728289,10.));
#17086=CARTESIAN_POINT('',(209.868752181296,39.8065050734778,10.));
#17087=CARTESIAN_POINT('',(209.868752181296,19.9032525367389,10.));
#17088=CARTESIAN_POINT('',(209.868752181296,44.7051656728289,12.));
#17089=CARTESIAN_POINT('',(209.868752181296,44.7051656728289,12.));
#17090=CARTESIAN_POINT('',(209.868752181296,39.8065050734778,12.));
#17091=CARTESIAN_POINT('',(209.868752181296,19.9032525367389,12.));
#17092=CARTESIAN_POINT('',(209.868752181296,39.8065050734778,12.));
#17093=CARTESIAN_POINT('Origin',(211.368752181296,39.8065050734778,12.));
#17094=CARTESIAN_POINT('',(212.868752181296,39.8065050734778,10.));
#17095=CARTESIAN_POINT('Origin',(211.368752181296,39.8065050734778,10.));
#17096=CARTESIAN_POINT('',(212.868752181296,39.8065050734778,12.));
#17097=CARTESIAN_POINT('Origin',(211.368752181296,39.8065050734778,12.));
#17098=CARTESIAN_POINT('',(212.868752181296,39.8065050734778,12.));
#17099=CARTESIAN_POINT('Origin',(212.868752181296,44.7051656728289,12.));
#17100=CARTESIAN_POINT('',(212.868752181296,44.7051656728289,10.));
#17101=CARTESIAN_POINT('',(212.868752181296,22.3525828364145,10.));
#17102=CARTESIAN_POINT('',(212.868752181296,44.7051656728289,12.));
#17103=CARTESIAN_POINT('',(212.868752181296,22.3525828364145,12.));
#17104=CARTESIAN_POINT('',(212.868752181296,44.7051656728289,12.));
#17105=CARTESIAN_POINT('Origin',(211.368752181296,44.7051656728289,12.));
#17106=CARTESIAN_POINT('Origin',(211.368752181296,44.7051656728289,10.));
#17107=CARTESIAN_POINT('Origin',(211.368752181296,44.7051656728289,12.));
#17108=CARTESIAN_POINT('Origin',(209.868752181296,5.29483432717106,12.));
#17109=CARTESIAN_POINT('',(209.868752181296,10.1934949265222,10.));
#17110=CARTESIAN_POINT('',(209.868752181296,5.29483432717106,10.));
#17111=CARTESIAN_POINT('',(209.868752181296,2.64741716358553,10.));
#17112=CARTESIAN_POINT('',(209.868752181296,10.1934949265222,12.));
#17113=CARTESIAN_POINT('',(209.868752181296,10.1934949265222,12.));
#17114=CARTESIAN_POINT('',(209.868752181296,5.29483432717106,12.));
#17115=CARTESIAN_POINT('',(209.868752181296,2.64741716358553,12.));
#17116=CARTESIAN_POINT('',(209.868752181296,5.29483432717106,12.));
#17117=CARTESIAN_POINT('Origin',(211.368752181296,5.29483432717106,12.));
#17118=CARTESIAN_POINT('',(212.868752181296,5.29483432717106,10.));
#17119=CARTESIAN_POINT('Origin',(211.368752181296,5.29483432717106,10.));
#17120=CARTESIAN_POINT('',(212.868752181296,5.29483432717106,12.));
#17121=CARTESIAN_POINT('Origin',(211.368752181296,5.29483432717106,12.));
#17122=CARTESIAN_POINT('',(212.868752181296,5.29483432717106,12.));
#17123=CARTESIAN_POINT('Origin',(212.868752181296,10.1934949265222,12.));
#17124=CARTESIAN_POINT('',(212.868752181296,10.1934949265222,10.));
#17125=CARTESIAN_POINT('',(212.868752181296,5.09674746326108,10.));
#17126=CARTESIAN_POINT('',(212.868752181296,10.1934949265222,12.));
#17127=CARTESIAN_POINT('',(212.868752181296,5.09674746326108,12.));
#17128=CARTESIAN_POINT('',(212.868752181296,10.1934949265222,12.));
#17129=CARTESIAN_POINT('Origin',(211.368752181296,10.1934949265222,12.));
#17130=CARTESIAN_POINT('Origin',(211.368752181296,10.1934949265222,10.));
#17131=CARTESIAN_POINT('Origin',(211.368752181296,10.1934949265222,12.));
#17132=CARTESIAN_POINT('Origin',(159.717862598919,11.70240347792,12.));
#17133=CARTESIAN_POINT('',(162.217862598919,11.70240347792,12.));
#17134=CARTESIAN_POINT('Origin',(159.717862598919,11.70240347792,12.));
#17135=CARTESIAN_POINT('',(162.217862598919,11.70240347792,10.));
#17136=CARTESIAN_POINT('',(162.217862598919,11.70240347792,12.));
#17137=CARTESIAN_POINT('Origin',(159.717862598919,11.70240347792,10.));
#17138=CARTESIAN_POINT('Origin',(186.130752874785,11.70240347792,12.));
#17139=CARTESIAN_POINT('',(188.630752874785,11.70240347792,12.));
#17140=CARTESIAN_POINT('Origin',(186.130752874785,11.70240347792,12.));
#17141=CARTESIAN_POINT('',(188.630752874785,11.70240347792,10.));
#17142=CARTESIAN_POINT('',(188.630752874785,11.70240347792,12.));
#17143=CARTESIAN_POINT('Origin',(186.130752874785,11.70240347792,10.));
#17144=CARTESIAN_POINT('Origin',(186.130752874785,38.29759652208,12.));
#17145=CARTESIAN_POINT('',(188.630752874785,38.29759652208,12.));
#17146=CARTESIAN_POINT('Origin',(186.130752874785,38.29759652208,12.));
#17147=CARTESIAN_POINT('',(188.630752874785,38.29759652208,10.));
#17148=CARTESIAN_POINT('',(188.630752874785,38.29759652208,12.));
#17149=CARTESIAN_POINT('Origin',(186.130752874785,38.29759652208,10.));
#17150=CARTESIAN_POINT('Origin',(159.717862598919,38.29759652208,12.));
#17151=CARTESIAN_POINT('',(162.217862598919,38.29759652208,12.));
#17152=CARTESIAN_POINT('Origin',(159.717862598919,38.29759652208,12.));
#17153=CARTESIAN_POINT('',(162.217862598919,38.29759652208,10.));
#17154=CARTESIAN_POINT('',(162.217862598919,38.29759652208,12.));
#17155=CARTESIAN_POINT('Origin',(159.717862598919,38.29759652208,10.));
#17156=CARTESIAN_POINT('Origin',(172.924307736852,25.,12.));
#17157=CARTESIAN_POINT('',(182.924307736852,25.,12.));
#17158=CARTESIAN_POINT('Origin',(172.924307736852,25.,12.));
#17159=CARTESIAN_POINT('',(182.924307736852,25.,10.));
#17160=CARTESIAN_POINT('',(182.924307736852,25.,12.));
#17161=CARTESIAN_POINT('Origin',(172.924307736852,25.,10.));
#17162=CARTESIAN_POINT('Origin',(171.424307736852,39.8065050734778,12.));
#17163=CARTESIAN_POINT('',(171.424307736852,44.7051656728289,10.));
#17164=CARTESIAN_POINT('',(171.424307736852,39.8065050734778,10.));
#17165=CARTESIAN_POINT('',(171.424307736852,19.9032525367389,10.));
#17166=CARTESIAN_POINT('',(171.424307736852,44.7051656728289,12.));
#17167=CARTESIAN_POINT('',(171.424307736852,44.7051656728289,12.));
#17168=CARTESIAN_POINT('',(171.424307736852,39.8065050734778,12.));
#17169=CARTESIAN_POINT('',(171.424307736852,19.9032525367389,12.));
#17170=CARTESIAN_POINT('',(171.424307736852,39.8065050734778,12.));
#17171=CARTESIAN_POINT('Origin',(172.924307736852,39.8065050734778,12.));
#17172=CARTESIAN_POINT('',(174.424307736852,39.8065050734778,10.));
#17173=CARTESIAN_POINT('Origin',(172.924307736852,39.8065050734778,10.));
#17174=CARTESIAN_POINT('',(174.424307736852,39.8065050734778,12.));
#17175=CARTESIAN_POINT('Origin',(172.924307736852,39.8065050734778,12.));
#17176=CARTESIAN_POINT('',(174.424307736852,39.8065050734778,12.));
#17177=CARTESIAN_POINT('Origin',(174.424307736852,44.7051656728289,12.));
#17178=CARTESIAN_POINT('',(174.424307736852,44.7051656728289,10.));
#17179=CARTESIAN_POINT('',(174.424307736852,22.3525828364145,10.));
#17180=CARTESIAN_POINT('',(174.424307736852,44.7051656728289,12.));
#17181=CARTESIAN_POINT('',(174.424307736852,22.3525828364145,12.));
#17182=CARTESIAN_POINT('',(174.424307736852,44.7051656728289,12.));
#17183=CARTESIAN_POINT('Origin',(172.924307736852,44.7051656728289,12.));
#17184=CARTESIAN_POINT('Origin',(172.924307736852,44.7051656728289,10.));
#17185=CARTESIAN_POINT('Origin',(172.924307736852,44.7051656728289,12.));
#17186=CARTESIAN_POINT('Origin',(171.424307736852,5.29483432717106,12.));
#17187=CARTESIAN_POINT('',(171.424307736852,10.1934949265222,10.));
#17188=CARTESIAN_POINT('',(171.424307736852,5.29483432717106,10.));
#17189=CARTESIAN_POINT('',(171.424307736852,2.64741716358553,10.));
#17190=CARTESIAN_POINT('',(171.424307736852,10.1934949265222,12.));
#17191=CARTESIAN_POINT('',(171.424307736852,10.1934949265222,12.));
#17192=CARTESIAN_POINT('',(171.424307736852,5.29483432717106,12.));
#17193=CARTESIAN_POINT('',(171.424307736852,2.64741716358553,12.));
#17194=CARTESIAN_POINT('',(171.424307736852,5.29483432717106,12.));
#17195=CARTESIAN_POINT('Origin',(172.924307736852,5.29483432717106,12.));
#17196=CARTESIAN_POINT('',(174.424307736852,5.29483432717106,10.));
#17197=CARTESIAN_POINT('Origin',(172.924307736852,5.29483432717106,10.));
#17198=CARTESIAN_POINT('',(174.424307736852,5.29483432717106,12.));
#17199=CARTESIAN_POINT('Origin',(172.924307736852,5.29483432717106,12.));
#17200=CARTESIAN_POINT('',(174.424307736852,5.29483432717106,12.));
#17201=CARTESIAN_POINT('Origin',(174.424307736852,10.1934949265222,12.));
#17202=CARTESIAN_POINT('',(174.424307736852,10.1934949265222,10.));
#17203=CARTESIAN_POINT('',(174.424307736852,5.09674746326108,10.));
#17204=CARTESIAN_POINT('',(174.424307736852,10.1934949265222,12.));
#17205=CARTESIAN_POINT('',(174.424307736852,5.09674746326108,12.));
#17206=CARTESIAN_POINT('',(174.424307736852,10.1934949265222,12.));
#17207=CARTESIAN_POINT('Origin',(172.924307736852,10.1934949265222,12.));
#17208=CARTESIAN_POINT('Origin',(172.924307736852,10.1934949265222,10.));
#17209=CARTESIAN_POINT('Origin',(172.924307736852,10.1934949265222,12.));
#17210=CARTESIAN_POINT('Origin',(121.273418154474,11.70240347792,12.));
#17211=CARTESIAN_POINT('',(123.773418154474,11.70240347792,12.));
#17212=CARTESIAN_POINT('Origin',(121.273418154474,11.70240347792,12.));
#17213=CARTESIAN_POINT('',(123.773418154474,11.70240347792,10.));
#17214=CARTESIAN_POINT('',(123.773418154474,11.70240347792,12.));
#17215=CARTESIAN_POINT('Origin',(121.273418154474,11.70240347792,10.));
#17216=CARTESIAN_POINT('Origin',(147.686308430341,11.70240347792,12.));
#17217=CARTESIAN_POINT('',(150.186308430341,11.70240347792,12.));
#17218=CARTESIAN_POINT('Origin',(147.686308430341,11.70240347792,12.));
#17219=CARTESIAN_POINT('',(150.186308430341,11.70240347792,10.));
#17220=CARTESIAN_POINT('',(150.186308430341,11.70240347792,12.));
#17221=CARTESIAN_POINT('Origin',(147.686308430341,11.70240347792,10.));
#17222=CARTESIAN_POINT('Origin',(147.686308430341,38.29759652208,12.));
#17223=CARTESIAN_POINT('',(150.186308430341,38.29759652208,12.));
#17224=CARTESIAN_POINT('Origin',(147.686308430341,38.29759652208,12.));
#17225=CARTESIAN_POINT('',(150.186308430341,38.29759652208,10.));
#17226=CARTESIAN_POINT('',(150.186308430341,38.29759652208,12.));
#17227=CARTESIAN_POINT('Origin',(147.686308430341,38.29759652208,10.));
#17228=CARTESIAN_POINT('Origin',(121.273418154474,38.29759652208,12.));
#17229=CARTESIAN_POINT('',(123.773418154474,38.29759652208,12.));
#17230=CARTESIAN_POINT('Origin',(121.273418154474,38.29759652208,12.));
#17231=CARTESIAN_POINT('',(123.773418154474,38.29759652208,10.));
#17232=CARTESIAN_POINT('',(123.773418154474,38.29759652208,12.));
#17233=CARTESIAN_POINT('Origin',(121.273418154474,38.29759652208,10.));
#17234=CARTESIAN_POINT('Origin',(134.479863292407,25.,12.));
#17235=CARTESIAN_POINT('',(144.479863292407,25.,12.));
#17236=CARTESIAN_POINT('Origin',(134.479863292407,25.,12.));
#17237=CARTESIAN_POINT('',(144.479863292407,25.,10.));
#17238=CARTESIAN_POINT('',(144.479863292407,25.,12.));
#17239=CARTESIAN_POINT('Origin',(134.479863292407,25.,10.));
#17240=CARTESIAN_POINT('Origin',(132.979863292407,39.8065050734778,12.));
#17241=CARTESIAN_POINT('',(132.979863292407,44.7051656728289,10.));
#17242=CARTESIAN_POINT('',(132.979863292407,39.8065050734778,10.));
#17243=CARTESIAN_POINT('',(132.979863292407,19.9032525367389,10.));
#17244=CARTESIAN_POINT('',(132.979863292407,44.7051656728289,12.));
#17245=CARTESIAN_POINT('',(132.979863292407,44.7051656728289,12.));
#17246=CARTESIAN_POINT('',(132.979863292407,39.8065050734778,12.));
#17247=CARTESIAN_POINT('',(132.979863292407,19.9032525367389,12.));
#17248=CARTESIAN_POINT('',(132.979863292407,39.8065050734778,12.));
#17249=CARTESIAN_POINT('Origin',(134.479863292407,39.8065050734778,12.));
#17250=CARTESIAN_POINT('',(135.979863292407,39.8065050734778,10.));
#17251=CARTESIAN_POINT('Origin',(134.479863292407,39.8065050734778,10.));
#17252=CARTESIAN_POINT('',(135.979863292407,39.8065050734778,12.));
#17253=CARTESIAN_POINT('Origin',(134.479863292407,39.8065050734778,12.));
#17254=CARTESIAN_POINT('',(135.979863292407,39.8065050734778,12.));
#17255=CARTESIAN_POINT('Origin',(135.979863292407,44.7051656728289,12.));
#17256=CARTESIAN_POINT('',(135.979863292407,44.7051656728289,10.));
#17257=CARTESIAN_POINT('',(135.979863292407,22.3525828364145,10.));
#17258=CARTESIAN_POINT('',(135.979863292407,44.7051656728289,12.));
#17259=CARTESIAN_POINT('',(135.979863292407,22.3525828364145,12.));
#17260=CARTESIAN_POINT('',(135.979863292407,44.7051656728289,12.));
#17261=CARTESIAN_POINT('Origin',(134.479863292407,44.7051656728289,12.));
#17262=CARTESIAN_POINT('Origin',(134.479863292407,44.7051656728289,10.));
#17263=CARTESIAN_POINT('Origin',(134.479863292407,44.7051656728289,12.));
#17264=CARTESIAN_POINT('Origin',(132.979863292407,5.29483432717106,12.));
#17265=CARTESIAN_POINT('',(132.979863292407,10.1934949265222,10.));
#17266=CARTESIAN_POINT('',(132.979863292407,5.29483432717106,10.));
#17267=CARTESIAN_POINT('',(132.979863292407,2.64741716358553,10.));
#17268=CARTESIAN_POINT('',(132.979863292407,10.1934949265222,12.));
#17269=CARTESIAN_POINT('',(132.979863292407,10.1934949265222,12.));
#17270=CARTESIAN_POINT('',(132.979863292407,5.29483432717106,12.));
#17271=CARTESIAN_POINT('',(132.979863292407,2.64741716358553,12.));
#17272=CARTESIAN_POINT('',(132.979863292407,5.29483432717106,12.));
#17273=CARTESIAN_POINT('Origin',(134.479863292407,5.29483432717106,12.));
#17274=CARTESIAN_POINT('',(135.979863292407,5.29483432717106,10.));
#17275=CARTESIAN_POINT('Origin',(134.479863292407,5.29483432717106,10.));
#17276=CARTESIAN_POINT('',(135.979863292407,5.29483432717106,12.));
#17277=CARTESIAN_POINT('Origin',(134.479863292407,5.29483432717106,12.));
#17278=CARTESIAN_POINT('',(135.979863292407,5.29483432717106,12.));
#17279=CARTESIAN_POINT('Origin',(135.979863292407,10.1934949265222,12.));
#17280=CARTESIAN_POINT('',(135.979863292407,10.1934949265222,10.));
#17281=CARTESIAN_POINT('',(135.979863292407,5.09674746326108,10.));
#17282=CARTESIAN_POINT('',(135.979863292407,10.1934949265222,12.));
#17283=CARTESIAN_POINT('',(135.979863292407,5.09674746326108,12.));
#17284=CARTESIAN_POINT('',(135.979863292407,10.1934949265222,12.));
#17285=CARTESIAN_POINT('Origin',(134.479863292407,10.1934949265222,12.));
#17286=CARTESIAN_POINT('Origin',(134.479863292407,10.1934949265222,10.));
#17287=CARTESIAN_POINT('Origin',(134.479863292407,10.1934949265222,12.));
#17288=CARTESIAN_POINT('Origin',(82.8289737100297,11.70240347792,12.));
#17289=CARTESIAN_POINT('',(85.3289737100297,11.70240347792,12.));
#17290=CARTESIAN_POINT('Origin',(82.8289737100297,11.70240347792,12.));
#17291=CARTESIAN_POINT('',(85.3289737100297,11.70240347792,10.));
#17292=CARTESIAN_POINT('',(85.3289737100297,11.70240347792,12.));
#17293=CARTESIAN_POINT('Origin',(82.8289737100297,11.70240347792,10.));
#17294=CARTESIAN_POINT('Origin',(109.241863985896,11.70240347792,12.));
#17295=CARTESIAN_POINT('',(111.741863985896,11.70240347792,12.));
#17296=CARTESIAN_POINT('Origin',(109.241863985896,11.70240347792,12.));
#17297=CARTESIAN_POINT('',(111.741863985896,11.70240347792,10.));
#17298=CARTESIAN_POINT('',(111.741863985896,11.70240347792,12.));
#17299=CARTESIAN_POINT('Origin',(109.241863985896,11.70240347792,10.));
#17300=CARTESIAN_POINT('Origin',(109.241863985896,38.29759652208,12.));
#17301=CARTESIAN_POINT('',(111.741863985896,38.29759652208,12.));
#17302=CARTESIAN_POINT('Origin',(109.241863985896,38.29759652208,12.));
#17303=CARTESIAN_POINT('',(111.741863985896,38.29759652208,10.));
#17304=CARTESIAN_POINT('',(111.741863985896,38.29759652208,12.));
#17305=CARTESIAN_POINT('Origin',(109.241863985896,38.29759652208,10.));
#17306=CARTESIAN_POINT('Origin',(82.8289737100297,38.29759652208,12.));
#17307=CARTESIAN_POINT('',(85.3289737100297,38.29759652208,12.));
#17308=CARTESIAN_POINT('Origin',(82.8289737100297,38.29759652208,12.));
#17309=CARTESIAN_POINT('',(85.3289737100297,38.29759652208,10.));
#17310=CARTESIAN_POINT('',(85.3289737100297,38.29759652208,12.));
#17311=CARTESIAN_POINT('Origin',(82.8289737100297,38.29759652208,10.));
#17312=CARTESIAN_POINT('Origin',(96.0354188479629,25.,12.));
#17313=CARTESIAN_POINT('',(106.035418847963,25.,12.));
#17314=CARTESIAN_POINT('Origin',(96.0354188479629,25.,12.));
#17315=CARTESIAN_POINT('',(106.035418847963,25.,10.));
#17316=CARTESIAN_POINT('',(106.035418847963,25.,12.));
#17317=CARTESIAN_POINT('Origin',(96.0354188479629,25.,10.));
#17318=CARTESIAN_POINT('Origin',(94.5354188479629,39.8065050734778,12.));
#17319=CARTESIAN_POINT('',(94.5354188479629,44.7051656728289,10.));
#17320=CARTESIAN_POINT('',(94.5354188479629,39.8065050734778,10.));
#17321=CARTESIAN_POINT('',(94.5354188479629,19.9032525367389,10.));
#17322=CARTESIAN_POINT('',(94.5354188479629,44.7051656728289,12.));
#17323=CARTESIAN_POINT('',(94.5354188479629,44.7051656728289,12.));
#17324=CARTESIAN_POINT('',(94.5354188479629,39.8065050734778,12.));
#17325=CARTESIAN_POINT('',(94.5354188479629,19.9032525367389,12.));
#17326=CARTESIAN_POINT('',(94.5354188479629,39.8065050734778,12.));
#17327=CARTESIAN_POINT('Origin',(96.0354188479629,39.8065050734778,12.));
#17328=CARTESIAN_POINT('',(97.5354188479629,39.8065050734778,10.));
#17329=CARTESIAN_POINT('Origin',(96.0354188479629,39.8065050734778,10.));
#17330=CARTESIAN_POINT('',(97.5354188479629,39.8065050734778,12.));
#17331=CARTESIAN_POINT('Origin',(96.0354188479629,39.8065050734778,12.));
#17332=CARTESIAN_POINT('',(97.5354188479629,39.8065050734778,12.));
#17333=CARTESIAN_POINT('Origin',(97.5354188479629,44.7051656728289,12.));
#17334=CARTESIAN_POINT('',(97.5354188479629,44.7051656728289,10.));
#17335=CARTESIAN_POINT('',(97.5354188479629,22.3525828364145,10.));
#17336=CARTESIAN_POINT('',(97.5354188479629,44.7051656728289,12.));
#17337=CARTESIAN_POINT('',(97.5354188479629,22.3525828364145,12.));
#17338=CARTESIAN_POINT('',(97.5354188479629,44.7051656728289,12.));
#17339=CARTESIAN_POINT('Origin',(96.0354188479629,44.7051656728289,12.));
#17340=CARTESIAN_POINT('Origin',(96.0354188479629,44.7051656728289,10.));
#17341=CARTESIAN_POINT('Origin',(96.0354188479629,44.7051656728289,12.));
#17342=CARTESIAN_POINT('Origin',(94.5354188479629,5.29483432717106,12.));
#17343=CARTESIAN_POINT('',(94.5354188479629,10.1934949265222,10.));
#17344=CARTESIAN_POINT('',(94.5354188479629,5.29483432717106,10.));
#17345=CARTESIAN_POINT('',(94.5354188479629,2.64741716358553,10.));
#17346=CARTESIAN_POINT('',(94.5354188479629,10.1934949265222,12.));
#17347=CARTESIAN_POINT('',(94.5354188479629,10.1934949265222,12.));
#17348=CARTESIAN_POINT('',(94.5354188479629,5.29483432717106,12.));
#17349=CARTESIAN_POINT('',(94.5354188479629,2.64741716358553,12.));
#17350=CARTESIAN_POINT('',(94.5354188479629,5.29483432717106,12.));
#17351=CARTESIAN_POINT('Origin',(96.0354188479629,5.29483432717106,12.));
#17352=CARTESIAN_POINT('',(97.5354188479629,5.29483432717106,10.));
#17353=CARTESIAN_POINT('Origin',(96.0354188479629,5.29483432717106,10.));
#17354=CARTESIAN_POINT('',(97.5354188479629,5.29483432717106,12.));
#17355=CARTESIAN_POINT('Origin',(96.0354188479629,5.29483432717106,12.));
#17356=CARTESIAN_POINT('',(97.5354188479629,5.29483432717106,12.));
#17357=CARTESIAN_POINT('Origin',(97.5354188479629,10.1934949265222,12.));
#17358=CARTESIAN_POINT('',(97.5354188479629,10.1934949265222,10.));
#17359=CARTESIAN_POINT('',(97.5354188479629,5.09674746326108,10.));
#17360=CARTESIAN_POINT('',(97.5354188479629,10.1934949265222,12.));
#17361=CARTESIAN_POINT('',(97.5354188479629,5.09674746326108,12.));
#17362=CARTESIAN_POINT('',(97.5354188479629,10.1934949265222,12.));
#17363=CARTESIAN_POINT('Origin',(96.0354188479629,10.1934949265222,12.));
#17364=CARTESIAN_POINT('Origin',(96.0354188479629,10.1934949265222,10.));
#17365=CARTESIAN_POINT('Origin',(96.0354188479629,10.1934949265222,12.));
#17366=CARTESIAN_POINT('Origin',(44.3845292655852,11.70240347792,12.));
#17367=CARTESIAN_POINT('',(46.8845292655852,11.70240347792,12.));
#17368=CARTESIAN_POINT('Origin',(44.3845292655852,11.70240347792,12.));
#17369=CARTESIAN_POINT('',(46.8845292655852,11.70240347792,10.));
#17370=CARTESIAN_POINT('',(46.8845292655852,11.70240347792,12.));
#17371=CARTESIAN_POINT('Origin',(44.3845292655852,11.70240347792,10.));
#17372=CARTESIAN_POINT('Origin',(70.7974195414516,11.70240347792,12.));
#17373=CARTESIAN_POINT('',(73.2974195414516,11.70240347792,12.));
#17374=CARTESIAN_POINT('Origin',(70.7974195414516,11.70240347792,12.));
#17375=CARTESIAN_POINT('',(73.2974195414516,11.70240347792,10.));
#17376=CARTESIAN_POINT('',(73.2974195414516,11.70240347792,12.));
#17377=CARTESIAN_POINT('Origin',(70.7974195414516,11.70240347792,10.));
#17378=CARTESIAN_POINT('Origin',(70.7974195414516,38.29759652208,12.));
#17379=CARTESIAN_POINT('',(73.2974195414516,38.29759652208,12.));
#17380=CARTESIAN_POINT('Origin',(70.7974195414516,38.29759652208,12.));
#17381=CARTESIAN_POINT('',(73.2974195414516,38.29759652208,10.));
#17382=CARTESIAN_POINT('',(73.2974195414516,38.29759652208,12.));
#17383=CARTESIAN_POINT('Origin',(70.7974195414516,38.29759652208,10.));
#17384=CARTESIAN_POINT('Origin',(44.3845292655852,38.29759652208,12.));
#17385=CARTESIAN_POINT('',(46.8845292655852,38.29759652208,12.));
#17386=CARTESIAN_POINT('Origin',(44.3845292655852,38.29759652208,12.));
#17387=CARTESIAN_POINT('',(46.8845292655852,38.29759652208,10.));
#17388=CARTESIAN_POINT('',(46.8845292655852,38.29759652208,12.));
#17389=CARTESIAN_POINT('Origin',(44.3845292655852,38.29759652208,10.));
#17390=CARTESIAN_POINT('Origin',(57.5909744035184,25.,12.));
#17391=CARTESIAN_POINT('',(67.5909744035184,25.,12.));
#17392=CARTESIAN_POINT('Origin',(57.5909744035184,25.,12.));
#17393=CARTESIAN_POINT('',(67.5909744035184,25.,10.));
#17394=CARTESIAN_POINT('',(67.5909744035184,25.,12.));
#17395=CARTESIAN_POINT('Origin',(57.5909744035184,25.,10.));
#17396=CARTESIAN_POINT('Origin',(56.0909744035184,39.8065050734778,12.));
#17397=CARTESIAN_POINT('',(56.0909744035184,44.7051656728289,10.));
#17398=CARTESIAN_POINT('',(56.0909744035184,39.8065050734778,10.));
#17399=CARTESIAN_POINT('',(56.0909744035185,19.9032525367389,10.));
#17400=CARTESIAN_POINT('',(56.0909744035184,44.7051656728289,12.));
#17401=CARTESIAN_POINT('',(56.0909744035184,44.7051656728289,12.));
#17402=CARTESIAN_POINT('',(56.0909744035184,39.8065050734778,12.));
#17403=CARTESIAN_POINT('',(56.0909744035184,19.9032525367389,12.));
#17404=CARTESIAN_POINT('',(56.0909744035184,39.8065050734778,12.));
#17405=CARTESIAN_POINT('Origin',(57.5909744035184,39.8065050734778,12.));
#17406=CARTESIAN_POINT('',(59.0909744035184,39.8065050734778,10.));
#17407=CARTESIAN_POINT('Origin',(57.5909744035184,39.8065050734778,10.));
#17408=CARTESIAN_POINT('',(59.0909744035184,39.8065050734778,12.));
#17409=CARTESIAN_POINT('Origin',(57.5909744035184,39.8065050734778,12.));
#17410=CARTESIAN_POINT('',(59.0909744035184,39.8065050734778,12.));
#17411=CARTESIAN_POINT('Origin',(59.0909744035184,44.7051656728289,12.));
#17412=CARTESIAN_POINT('',(59.0909744035184,44.7051656728289,10.));
#17413=CARTESIAN_POINT('',(59.0909744035184,22.3525828364145,10.));
#17414=CARTESIAN_POINT('',(59.0909744035184,44.7051656728289,12.));
#17415=CARTESIAN_POINT('',(59.0909744035184,22.3525828364145,12.));
#17416=CARTESIAN_POINT('',(59.0909744035184,44.7051656728289,12.));
#17417=CARTESIAN_POINT('Origin',(57.5909744035184,44.7051656728289,12.));
#17418=CARTESIAN_POINT('Origin',(57.5909744035184,44.7051656728289,10.));
#17419=CARTESIAN_POINT('Origin',(57.5909744035184,44.7051656728289,12.));
#17420=CARTESIAN_POINT('Origin',(56.0909744035184,5.29483432717106,12.));
#17421=CARTESIAN_POINT('',(56.0909744035184,10.1934949265222,10.));
#17422=CARTESIAN_POINT('',(56.0909744035184,5.29483432717106,10.));
#17423=CARTESIAN_POINT('',(56.0909744035185,2.64741716358553,10.));
#17424=CARTESIAN_POINT('',(56.0909744035184,10.1934949265222,12.));
#17425=CARTESIAN_POINT('',(56.0909744035184,10.1934949265222,12.));
#17426=CARTESIAN_POINT('',(56.0909744035184,5.29483432717106,12.));
#17427=CARTESIAN_POINT('',(56.0909744035184,2.64741716358553,12.));
#17428=CARTESIAN_POINT('',(56.0909744035184,5.29483432717106,12.));
#17429=CARTESIAN_POINT('Origin',(57.5909744035184,5.29483432717106,12.));
#17430=CARTESIAN_POINT('',(59.0909744035184,5.29483432717106,10.));
#17431=CARTESIAN_POINT('Origin',(57.5909744035184,5.29483432717106,10.));
#17432=CARTESIAN_POINT('',(59.0909744035184,5.29483432717106,12.));
#17433=CARTESIAN_POINT('Origin',(57.5909744035184,5.29483432717106,12.));
#17434=CARTESIAN_POINT('',(59.0909744035184,5.29483432717106,12.));
#17435=CARTESIAN_POINT('Origin',(59.0909744035184,10.1934949265222,12.));
#17436=CARTESIAN_POINT('',(59.0909744035184,10.1934949265222,10.));
#17437=CARTESIAN_POINT('',(59.0909744035184,5.09674746326108,10.));
#17438=CARTESIAN_POINT('',(59.0909744035184,10.1934949265222,12.));
#17439=CARTESIAN_POINT('',(59.0909744035184,5.09674746326108,12.));
#17440=CARTESIAN_POINT('',(59.0909744035184,10.1934949265222,12.));
#17441=CARTESIAN_POINT('Origin',(57.5909744035184,10.1934949265222,12.));
#17442=CARTESIAN_POINT('Origin',(57.5909744035184,10.1934949265222,10.));
#17443=CARTESIAN_POINT('Origin',(57.5909744035184,10.1934949265222,12.));
#17444=CARTESIAN_POINT('Origin',(32.3529750970072,11.70240347792,12.));
#17445=CARTESIAN_POINT('',(34.8529750970072,11.70240347792,12.));
#17446=CARTESIAN_POINT('Origin',(32.3529750970072,11.70240347792,12.));
#17447=CARTESIAN_POINT('',(34.8529750970072,11.70240347792,10.));
#17448=CARTESIAN_POINT('',(34.8529750970072,11.70240347792,12.));
#17449=CARTESIAN_POINT('Origin',(32.3529750970072,11.70240347792,10.));
#17450=CARTESIAN_POINT('Origin',(5.94008482114076,38.29759652208,12.));
#17451=CARTESIAN_POINT('',(8.44008482114076,38.29759652208,12.));
#17452=CARTESIAN_POINT('Origin',(5.94008482114076,38.29759652208,12.));
#17453=CARTESIAN_POINT('',(8.44008482114076,38.29759652208,10.));
#17454=CARTESIAN_POINT('',(8.44008482114076,38.29759652208,12.));
#17455=CARTESIAN_POINT('Origin',(5.94008482114076,38.29759652208,10.));
#17456=CARTESIAN_POINT('Origin',(17.646529959074,39.8065050734778,12.));
#17457=CARTESIAN_POINT('',(17.646529959074,44.7051656728289,10.));
#17458=CARTESIAN_POINT('',(17.646529959074,39.8065050734778,10.));
#17459=CARTESIAN_POINT('',(17.646529959074,19.9032525367389,10.));
#17460=CARTESIAN_POINT('',(17.646529959074,44.7051656728289,12.));
#17461=CARTESIAN_POINT('',(17.646529959074,44.7051656728289,12.));
#17462=CARTESIAN_POINT('',(17.646529959074,39.8065050734778,12.));
#17463=CARTESIAN_POINT('',(17.646529959074,19.9032525367389,12.));
#17464=CARTESIAN_POINT('',(17.646529959074,39.8065050734778,12.));
#17465=CARTESIAN_POINT('Origin',(19.146529959074,39.8065050734778,12.));
#17466=CARTESIAN_POINT('',(20.646529959074,39.8065050734778,10.));
#17467=CARTESIAN_POINT('Origin',(19.146529959074,39.8065050734778,10.));
#17468=CARTESIAN_POINT('',(20.646529959074,39.8065050734778,12.));
#17469=CARTESIAN_POINT('Origin',(19.146529959074,39.8065050734778,12.));
#17470=CARTESIAN_POINT('',(20.646529959074,39.8065050734778,12.));
#17471=CARTESIAN_POINT('Origin',(20.646529959074,44.7051656728289,12.));
#17472=CARTESIAN_POINT('',(20.646529959074,44.7051656728289,10.));
#17473=CARTESIAN_POINT('',(20.6465299590739,22.3525828364145,10.));
#17474=CARTESIAN_POINT('',(20.646529959074,44.7051656728289,12.));
#17475=CARTESIAN_POINT('',(20.646529959074,22.3525828364145,12.));
#17476=CARTESIAN_POINT('',(20.646529959074,44.7051656728289,12.));
#17477=CARTESIAN_POINT('Origin',(19.146529959074,44.7051656728289,12.));
#17478=CARTESIAN_POINT('Origin',(19.146529959074,44.7051656728289,10.));
#17479=CARTESIAN_POINT('Origin',(19.146529959074,44.7051656728289,12.));
#17480=CARTESIAN_POINT('Origin',(17.646529959074,5.29483432717106,12.));
#17481=CARTESIAN_POINT('',(17.646529959074,10.1934949265222,10.));
#17482=CARTESIAN_POINT('',(17.646529959074,5.29483432717106,10.));
#17483=CARTESIAN_POINT('',(17.646529959074,2.64741716358553,10.));
#17484=CARTESIAN_POINT('',(17.646529959074,10.1934949265222,12.));
#17485=CARTESIAN_POINT('',(17.646529959074,10.1934949265222,12.));
#17486=CARTESIAN_POINT('',(17.646529959074,5.29483432717106,12.));
#17487=CARTESIAN_POINT('',(17.646529959074,2.64741716358553,12.));
#17488=CARTESIAN_POINT('',(17.646529959074,5.29483432717106,12.));
#17489=CARTESIAN_POINT('Origin',(19.146529959074,5.29483432717106,12.));
#17490=CARTESIAN_POINT('',(20.646529959074,5.29483432717106,10.));
#17491=CARTESIAN_POINT('Origin',(19.146529959074,5.29483432717106,10.));
#17492=CARTESIAN_POINT('',(20.646529959074,5.29483432717106,12.));
#17493=CARTESIAN_POINT('Origin',(19.146529959074,5.29483432717106,12.));
#17494=CARTESIAN_POINT('',(20.646529959074,5.29483432717106,12.));
#17495=CARTESIAN_POINT('Origin',(20.646529959074,10.1934949265222,12.));
#17496=CARTESIAN_POINT('',(20.646529959074,10.1934949265222,10.));
#17497=CARTESIAN_POINT('',(20.6465299590739,5.09674746326108,10.));
#17498=CARTESIAN_POINT('',(20.646529959074,10.1934949265222,12.));
#17499=CARTESIAN_POINT('',(20.646529959074,5.09674746326108,12.));
#17500=CARTESIAN_POINT('',(20.646529959074,10.1934949265222,12.));
#17501=CARTESIAN_POINT('Origin',(19.146529959074,10.1934949265222,12.));
#17502=CARTESIAN_POINT('Origin',(19.146529959074,10.1934949265222,10.));
#17503=CARTESIAN_POINT('Origin',(19.146529959074,10.1934949265222,12.));
#17504=CARTESIAN_POINT('Origin',(19.146529959074,25.,12.));
#17505=CARTESIAN_POINT('',(29.146529959074,25.,12.));
#17506=CARTESIAN_POINT('Origin',(19.146529959074,25.,12.));
#17507=CARTESIAN_POINT('',(29.146529959074,25.,10.));
#17508=CARTESIAN_POINT('',(29.146529959074,25.,12.));
#17509=CARTESIAN_POINT('Origin',(19.146529959074,25.,10.));
#17510=CARTESIAN_POINT('Origin',(32.3529750970072,38.29759652208,12.));
#17511=CARTESIAN_POINT('',(34.8529750970072,38.29759652208,12.));
#17512=CARTESIAN_POINT('Origin',(32.3529750970072,38.29759652208,12.));
#17513=CARTESIAN_POINT('',(34.8529750970072,38.29759652208,10.));
#17514=CARTESIAN_POINT('',(34.8529750970072,38.29759652208,12.));
#17515=CARTESIAN_POINT('Origin',(32.3529750970072,38.29759652208,10.));
#17516=CARTESIAN_POINT('Origin',(5.94008482114076,11.70240347792,12.));
#17517=CARTESIAN_POINT('',(8.44008482114076,11.70240347792,12.));
#17518=CARTESIAN_POINT('Origin',(5.94008482114076,11.70240347792,12.));
#17519=CARTESIAN_POINT('',(8.44008482114076,11.70240347792,10.));
#17520=CARTESIAN_POINT('',(8.44008482114076,11.70240347792,12.));
#17521=CARTESIAN_POINT('Origin',(5.94008482114076,11.70240347792,10.));
#17522=CARTESIAN_POINT('Origin',(288.,2.5,9.5));
#17523=CARTESIAN_POINT('',(0.,2.,9.5));
#17524=CARTESIAN_POINT('',(0.,2.5,10.));
#17525=CARTESIAN_POINT('Origin',(0.,2.5,9.5));
#17526=CARTESIAN_POINT('',(384.,2.5,10.));
#17527=CARTESIAN_POINT('',(288.,2.5,10.));
#17528=CARTESIAN_POINT('',(384.,2.,9.5));
#17529=CARTESIAN_POINT('Origin',(384.,2.5,9.5));
#17530=CARTESIAN_POINT('',(288.,2.,9.5));
#17531=CARTESIAN_POINT('Origin',(384.,0.,10.));
#17532=CARTESIAN_POINT('',(0.,47.5,10.));
#17533=CARTESIAN_POINT('',(0.,0.,10.));
#17534=CARTESIAN_POINT('',(384.,47.5,10.));
#17535=CARTESIAN_POINT('',(288.,47.5,10.));
#17536=CARTESIAN_POINT('',(384.,0.,10.));
#17537=CARTESIAN_POINT('Origin',(288.,47.5,9.5));
#17538=CARTESIAN_POINT('',(0.,48.,9.5));
#17539=CARTESIAN_POINT('Origin',(0.,47.5,9.5));
#17540=CARTESIAN_POINT('',(384.,48.,9.5));
#17541=CARTESIAN_POINT('',(288.,48.,9.5));
#17542=CARTESIAN_POINT('Origin',(384.,47.5,9.5));
#17543=CARTESIAN_POINT('Origin',(192.,48.,5.));
#17544=CARTESIAN_POINT('',(0.,48.,0.));
#17545=CARTESIAN_POINT('',(0.,48.,12.));
#17546=CARTESIAN_POINT('',(384.,48.,0.));
#17547=CARTESIAN_POINT('',(0.,48.,0.));
#17548=CARTESIAN_POINT('',(384.,48.,0.));
#17549=CARTESIAN_POINT('',(6.02178569715406,48.,3.89451831659521));
#17550=CARTESIAN_POINT('Origin',(8.02178569715406,48.,3.89451831659521));
#17551=CARTESIAN_POINT('',(302.021785697154,48.,3.89451831659521));
#17552=CARTESIAN_POINT('Origin',(304.021785697154,48.,3.89451831659521));
#17553=CARTESIAN_POINT('',(358.021785697154,48.,3.89451831659521));
#17554=CARTESIAN_POINT('Origin',(360.021785697154,48.,3.89451831659521));
#17555=CARTESIAN_POINT('',(206.021785697154,48.,3.89451831659521));
#17556=CARTESIAN_POINT('Origin',(208.021785697154,48.,3.89451831659521));
#17557=CARTESIAN_POINT('',(374.021785697154,48.,3.89451831659521));
#17558=CARTESIAN_POINT('Origin',(376.021785697154,48.,3.89451831659521));
#17559=CARTESIAN_POINT('',(14.0217856971541,48.,3.89451831659521));
#17560=CARTESIAN_POINT('Origin',(16.0217856971541,48.,3.89451831659521));
#17561=CARTESIAN_POINT('',(182.021785697154,48.,3.89451831659521));
#17562=CARTESIAN_POINT('Origin',(184.021785697154,48.,3.89451831659521));
#17563=CARTESIAN_POINT('',(118.021785697154,48.,3.89451831659521));
#17564=CARTESIAN_POINT('Origin',(120.021785697154,48.,3.89451831659521));
#17565=CARTESIAN_POINT('',(126.021785697154,48.,3.89451831659521));
#17566=CARTESIAN_POINT('Origin',(128.021785697154,48.,3.89451831659521));
#17567=CARTESIAN_POINT('',(278.021785697154,48.,3.89451831659521));
#17568=CARTESIAN_POINT('Origin',(280.021785697154,48.,3.89451831659521));
#17569=CARTESIAN_POINT('',(94.0217856971541,48.,3.89451831659521));
#17570=CARTESIAN_POINT('Origin',(96.0217856971541,48.,3.89451831659521));
#17571=CARTESIAN_POINT('',(198.021785697154,48.,3.89451831659521));
#17572=CARTESIAN_POINT('Origin',(200.021785697154,48.,3.89451831659521));
#17573=CARTESIAN_POINT('',(70.0217856971541,48.,3.89451831659521));
#17574=CARTESIAN_POINT('Origin',(72.0217856971541,48.,3.89451831659521));
#17575=CARTESIAN_POINT('',(214.021785697154,48.,3.89451831659521));
#17576=CARTESIAN_POINT('Origin',(216.021785697154,48.,3.89451831659521));
#17577=CARTESIAN_POINT('',(246.021785697154,48.,3.89451831659521));
#17578=CARTESIAN_POINT('Origin',(248.021785697154,48.,3.89451831659521));
#17579=CARTESIAN_POINT('',(78.0217856971541,48.,3.89451831659521));
#17580=CARTESIAN_POINT('Origin',(80.0217856971541,48.,3.89451831659521));
#17581=CARTESIAN_POINT('',(262.021785697154,48.,3.89451831659521));
#17582=CARTESIAN_POINT('Origin',(264.021785697154,48.,3.89451831659521));
#17583=CARTESIAN_POINT('',(46.0217856971541,48.,3.89451831659521));
#17584=CARTESIAN_POINT('Origin',(48.0217856971541,48.,3.89451831659521));
#17585=CARTESIAN_POINT('',(30.0217856971541,48.,3.89451831659521));
#17586=CARTESIAN_POINT('Origin',(32.0217856971541,48.,3.89451831659521));
#17587=CARTESIAN_POINT('',(334.021785697154,48.,3.89451831659521));
#17588=CARTESIAN_POINT('Origin',(336.021785697154,48.,3.89451831659521));
#17589=CARTESIAN_POINT('',(38.0217856971541,48.,3.89451831659521));
#17590=CARTESIAN_POINT('Origin',(40.0217856971541,48.,3.89451831659521));
#17591=CARTESIAN_POINT('',(102.021785697154,48.,3.89451831659521));
#17592=CARTESIAN_POINT('Origin',(104.021785697154,48.,3.89451831659521));
#17593=CARTESIAN_POINT('',(62.0217856971541,48.,3.89451831659521));
#17594=CARTESIAN_POINT('Origin',(64.0217856971541,48.,3.89451831659521));
#17595=CARTESIAN_POINT('',(286.021785697154,48.,3.89451831659521));
#17596=CARTESIAN_POINT('Origin',(288.021785697154,48.,3.89451831659521));
#17597=CARTESIAN_POINT('',(134.021785697154,48.,3.89451831659521));
#17598=CARTESIAN_POINT('Origin',(136.021785697154,48.,3.89451831659521));
#17599=CARTESIAN_POINT('',(110.021785697154,48.,3.89451831659521));
#17600=CARTESIAN_POINT('Origin',(112.021785697154,48.,3.89451831659521));
#17601=CARTESIAN_POINT('',(174.021785697154,48.,3.89451831659521));
#17602=CARTESIAN_POINT('Origin',(176.021785697154,48.,3.89451831659521));
#17603=CARTESIAN_POINT('',(166.021785697154,48.,3.89451831659521));
#17604=CARTESIAN_POINT('Origin',(168.021785697154,48.,3.89451831659521));
#17605=CARTESIAN_POINT('',(158.021785697154,48.,3.89451831659521));
#17606=CARTESIAN_POINT('Origin',(160.021785697154,48.,3.89451831659521));
#17607=CARTESIAN_POINT('',(86.0217856971541,48.,3.89451831659521));
#17608=CARTESIAN_POINT('Origin',(88.0217856971541,48.,3.89451831659521));
#17609=CARTESIAN_POINT('',(22.0217856971541,48.,3.89451831659521));
#17610=CARTESIAN_POINT('Origin',(24.0217856971541,48.,3.89451831659521));
#17611=CARTESIAN_POINT('',(318.021785697154,48.,3.89451831659521));
#17612=CARTESIAN_POINT('Origin',(320.021785697154,48.,3.89451831659521));
#17613=CARTESIAN_POINT('',(190.021785697154,48.,3.89451831659521));
#17614=CARTESIAN_POINT('Origin',(192.021785697154,48.,3.89451831659521));
#17615=CARTESIAN_POINT('',(230.021785697154,48.,3.89451831659521));
#17616=CARTESIAN_POINT('Origin',(232.021785697154,48.,3.89451831659521));
#17617=CARTESIAN_POINT('',(270.021785697154,48.,3.89451831659521));
#17618=CARTESIAN_POINT('Origin',(272.021785697154,48.,3.89451831659521));
#17619=CARTESIAN_POINT('',(238.021785697154,48.,3.89451831659521));
#17620=CARTESIAN_POINT('Origin',(240.021785697154,48.,3.89451831659521));
#17621=CARTESIAN_POINT('',(54.0217856971541,48.,3.89451831659521));
#17622=CARTESIAN_POINT('Origin',(56.0217856971541,48.,3.89451831659521));
#17623=CARTESIAN_POINT('',(350.021785697154,48.,3.89451831659521));
#17624=CARTESIAN_POINT('Origin',(352.021785697154,48.,3.89451831659521));
#17625=CARTESIAN_POINT('',(342.021785697154,48.,3.89451831659521));
#17626=CARTESIAN_POINT('Origin',(344.021785697154,48.,3.89451831659521));
#17627=CARTESIAN_POINT('',(326.021785697154,48.,3.89451831659521));
#17628=CARTESIAN_POINT('Origin',(328.021785697154,48.,3.89451831659521));
#17629=CARTESIAN_POINT('',(142.021785697154,48.,3.89451831659521));
#17630=CARTESIAN_POINT('Origin',(144.021785697154,48.,3.89451831659521));
#17631=CARTESIAN_POINT('',(150.021785697154,48.,3.89451831659521));
#17632=CARTESIAN_POINT('Origin',(152.021785697154,48.,3.89451831659521));
#17633=CARTESIAN_POINT('',(254.021785697154,48.,3.89451831659521));
#17634=CARTESIAN_POINT('Origin',(256.021785697154,48.,3.89451831659521));
#17635=CARTESIAN_POINT('',(366.021785697154,48.,3.89451831659521));
#17636=CARTESIAN_POINT('Origin',(368.021785697154,48.,3.89451831659521));
#17637=CARTESIAN_POINT('',(294.021785697154,48.,3.89451831659521));
#17638=CARTESIAN_POINT('Origin',(296.021785697154,48.,3.89451831659521));
#17639=CARTESIAN_POINT('',(222.021785697154,48.,3.89451831659521));
#17640=CARTESIAN_POINT('Origin',(224.021785697154,48.,3.89451831659521));
#17641=CARTESIAN_POINT('',(310.021785697154,48.,3.89451831659521));
#17642=CARTESIAN_POINT('Origin',(312.021785697154,48.,3.89451831659521));
#17643=CARTESIAN_POINT('Origin',(96.,48.,10.));
#17644=CARTESIAN_POINT('',(384.,48.,12.));
#17645=CARTESIAN_POINT('',(384.,50.,10.));
#17646=CARTESIAN_POINT('Origin',(384.,48.,10.));
#17647=CARTESIAN_POINT('',(0.,50.,10.));
#17648=CARTESIAN_POINT('',(96.,50.,10.));
#17649=CARTESIAN_POINT('',(0.,48.,12.));
#17650=CARTESIAN_POINT('Origin',(0.,48.,10.));
#17651=CARTESIAN_POINT('',(96.,48.,12.));
#17652=CARTESIAN_POINT('Origin',(0.,0.,12.));
#17653=CARTESIAN_POINT('',(0.,2.,12.));
#17654=CARTESIAN_POINT('',(0.,0.,12.));
#17655=CARTESIAN_POINT('',(384.,2.,12.));
#17656=CARTESIAN_POINT('',(96.,2.,12.));
#17657=CARTESIAN_POINT('',(384.,0.,12.));
#17658=CARTESIAN_POINT('Origin',(0.,0.,0.));
#17659=CARTESIAN_POINT('',(0.,50.,0.));
#17660=CARTESIAN_POINT('',(0.,50.,12.));
#17661=CARTESIAN_POINT('',(0.,48.,0.));
#17662=CARTESIAN_POINT('',(0.,2.,0.));
#17663=CARTESIAN_POINT('',(0.,2.,12.));
#17664=CARTESIAN_POINT('',(0.,0.,0.));
#17665=CARTESIAN_POINT('',(0.,0.,0.));
#17666=CARTESIAN_POINT('',(0.,0.,10.));
#17667=CARTESIAN_POINT('',(0.,0.,12.));
#17668=CARTESIAN_POINT('Origin',(0.,2.,10.));
#17669=CARTESIAN_POINT('Origin',(96.,2.,10.));
#17670=CARTESIAN_POINT('',(384.,0.,10.));
#17671=CARTESIAN_POINT('Origin',(384.,2.,10.));
#17672=CARTESIAN_POINT('',(96.,0.,10.));
#17673=CARTESIAN_POINT('Origin',(8.02178569715406,48.,3.89451831659521));
#17674=CARTESIAN_POINT('',(6.02178569715406,50.,3.89451831659521));
#17675=CARTESIAN_POINT('Origin',(8.02178569715406,50.,3.89451831659521));
#17676=CARTESIAN_POINT('',(6.02178569715406,48.,3.89451831659521));
#17677=CARTESIAN_POINT('Origin',(304.021785697154,48.,3.89451831659521));
#17678=CARTESIAN_POINT('',(302.021785697154,50.,3.89451831659521));
#17679=CARTESIAN_POINT('Origin',(304.021785697154,50.,3.89451831659521));
#17680=CARTESIAN_POINT('',(302.021785697154,48.,3.89451831659521));
#17681=CARTESIAN_POINT('Origin',(360.021785697154,48.,3.89451831659521));
#17682=CARTESIAN_POINT('',(358.021785697154,50.,3.89451831659521));
#17683=CARTESIAN_POINT('Origin',(360.021785697154,50.,3.89451831659521));
#17684=CARTESIAN_POINT('',(358.021785697154,48.,3.89451831659521));
#17685=CARTESIAN_POINT('Origin',(208.021785697154,48.,3.89451831659521));
#17686=CARTESIAN_POINT('',(206.021785697154,50.,3.89451831659521));
#17687=CARTESIAN_POINT('Origin',(208.021785697154,50.,3.89451831659521));
#17688=CARTESIAN_POINT('',(206.021785697154,48.,3.89451831659521));
#17689=CARTESIAN_POINT('Origin',(376.021785697154,48.,3.89451831659521));
#17690=CARTESIAN_POINT('',(374.021785697154,50.,3.89451831659521));
#17691=CARTESIAN_POINT('Origin',(376.021785697154,50.,3.89451831659521));
#17692=CARTESIAN_POINT('',(374.021785697154,48.,3.89451831659521));
#17693=CARTESIAN_POINT('Origin',(16.0217856971541,48.,3.89451831659521));
#17694=CARTESIAN_POINT('',(14.0217856971541,50.,3.89451831659521));
#17695=CARTESIAN_POINT('Origin',(16.0217856971541,50.,3.89451831659521));
#17696=CARTESIAN_POINT('',(14.0217856971541,48.,3.89451831659521));
#17697=CARTESIAN_POINT('Origin',(184.021785697154,48.,3.89451831659521));
#17698=CARTESIAN_POINT('',(182.021785697154,50.,3.89451831659521));
#17699=CARTESIAN_POINT('Origin',(184.021785697154,50.,3.89451831659521));
#17700=CARTESIAN_POINT('',(182.021785697154,48.,3.89451831659521));
#17701=CARTESIAN_POINT('Origin',(120.021785697154,48.,3.89451831659521));
#17702=CARTESIAN_POINT('',(118.021785697154,50.,3.89451831659521));
#17703=CARTESIAN_POINT('Origin',(120.021785697154,50.,3.89451831659521));
#17704=CARTESIAN_POINT('',(118.021785697154,48.,3.89451831659521));
#17705=CARTESIAN_POINT('Origin',(128.021785697154,48.,3.89451831659521));
#17706=CARTESIAN_POINT('',(126.021785697154,50.,3.89451831659521));
#17707=CARTESIAN_POINT('Origin',(128.021785697154,50.,3.89451831659521));
#17708=CARTESIAN_POINT('',(126.021785697154,48.,3.89451831659521));
#17709=CARTESIAN_POINT('Origin',(280.021785697154,48.,3.89451831659521));
#17710=CARTESIAN_POINT('',(278.021785697154,50.,3.89451831659521));
#17711=CARTESIAN_POINT('Origin',(280.021785697154,50.,3.89451831659521));
#17712=CARTESIAN_POINT('',(278.021785697154,48.,3.89451831659521));
#17713=CARTESIAN_POINT('Origin',(96.0217856971541,48.,3.89451831659521));
#17714=CARTESIAN_POINT('',(94.0217856971541,50.,3.89451831659521));
#17715=CARTESIAN_POINT('Origin',(96.0217856971541,50.,3.89451831659521));
#17716=CARTESIAN_POINT('',(94.0217856971541,48.,3.89451831659521));
#17717=CARTESIAN_POINT('Origin',(200.021785697154,48.,3.89451831659521));
#17718=CARTESIAN_POINT('',(198.021785697154,50.,3.89451831659521));
#17719=CARTESIAN_POINT('Origin',(200.021785697154,50.,3.89451831659521));
#17720=CARTESIAN_POINT('',(198.021785697154,48.,3.89451831659521));
#17721=CARTESIAN_POINT('Origin',(72.0217856971541,48.,3.89451831659521));
#17722=CARTESIAN_POINT('',(70.0217856971541,50.,3.89451831659521));
#17723=CARTESIAN_POINT('Origin',(72.0217856971541,50.,3.89451831659521));
#17724=CARTESIAN_POINT('',(70.0217856971541,48.,3.89451831659521));
#17725=CARTESIAN_POINT('Origin',(216.021785697154,48.,3.89451831659521));
#17726=CARTESIAN_POINT('',(214.021785697154,50.,3.89451831659521));
#17727=CARTESIAN_POINT('Origin',(216.021785697154,50.,3.89451831659521));
#17728=CARTESIAN_POINT('',(214.021785697154,48.,3.89451831659521));
#17729=CARTESIAN_POINT('Origin',(248.021785697154,48.,3.89451831659521));
#17730=CARTESIAN_POINT('',(246.021785697154,50.,3.89451831659521));
#17731=CARTESIAN_POINT('Origin',(248.021785697154,50.,3.89451831659521));
#17732=CARTESIAN_POINT('',(246.021785697154,48.,3.89451831659521));
#17733=CARTESIAN_POINT('Origin',(80.0217856971541,48.,3.89451831659521));
#17734=CARTESIAN_POINT('',(78.0217856971541,50.,3.89451831659521));
#17735=CARTESIAN_POINT('Origin',(80.0217856971541,50.,3.89451831659521));
#17736=CARTESIAN_POINT('',(78.0217856971541,48.,3.89451831659521));
#17737=CARTESIAN_POINT('Origin',(264.021785697154,48.,3.89451831659521));
#17738=CARTESIAN_POINT('',(262.021785697154,50.,3.89451831659521));
#17739=CARTESIAN_POINT('Origin',(264.021785697154,50.,3.89451831659521));
#17740=CARTESIAN_POINT('',(262.021785697154,48.,3.89451831659521));
#17741=CARTESIAN_POINT('Origin',(48.0217856971541,48.,3.89451831659521));
#17742=CARTESIAN_POINT('',(46.0217856971541,50.,3.89451831659521));
#17743=CARTESIAN_POINT('Origin',(48.0217856971541,50.,3.89451831659521));
#17744=CARTESIAN_POINT('',(46.0217856971541,48.,3.89451831659521));
#17745=CARTESIAN_POINT('Origin',(32.0217856971541,48.,3.89451831659521));
#17746=CARTESIAN_POINT('',(30.0217856971541,50.,3.89451831659521));
#17747=CARTESIAN_POINT('Origin',(32.0217856971541,50.,3.89451831659521));
#17748=CARTESIAN_POINT('',(30.0217856971541,48.,3.89451831659521));
#17749=CARTESIAN_POINT('Origin',(336.021785697154,48.,3.89451831659521));
#17750=CARTESIAN_POINT('',(334.021785697154,50.,3.89451831659521));
#17751=CARTESIAN_POINT('Origin',(336.021785697154,50.,3.89451831659521));
#17752=CARTESIAN_POINT('',(334.021785697154,48.,3.89451831659521));
#17753=CARTESIAN_POINT('Origin',(40.0217856971541,48.,3.89451831659521));
#17754=CARTESIAN_POINT('',(38.0217856971541,50.,3.89451831659521));
#17755=CARTESIAN_POINT('Origin',(40.0217856971541,50.,3.89451831659521));
#17756=CARTESIAN_POINT('',(38.0217856971541,48.,3.89451831659521));
#17757=CARTESIAN_POINT('Origin',(104.021785697154,48.,3.89451831659521));
#17758=CARTESIAN_POINT('',(102.021785697154,50.,3.89451831659521));
#17759=CARTESIAN_POINT('Origin',(104.021785697154,50.,3.89451831659521));
#17760=CARTESIAN_POINT('',(102.021785697154,48.,3.89451831659521));
#17761=CARTESIAN_POINT('Origin',(64.0217856971541,48.,3.89451831659521));
#17762=CARTESIAN_POINT('',(62.0217856971541,50.,3.89451831659521));
#17763=CARTESIAN_POINT('Origin',(64.0217856971541,50.,3.89451831659521));
#17764=CARTESIAN_POINT('',(62.0217856971541,48.,3.89451831659521));
#17765=CARTESIAN_POINT('Origin',(288.021785697154,48.,3.89451831659521));
#17766=CARTESIAN_POINT('',(286.021785697154,50.,3.89451831659521));
#17767=CARTESIAN_POINT('Origin',(288.021785697154,50.,3.89451831659521));
#17768=CARTESIAN_POINT('',(286.021785697154,48.,3.89451831659521));
#17769=CARTESIAN_POINT('Origin',(136.021785697154,48.,3.89451831659521));
#17770=CARTESIAN_POINT('',(134.021785697154,50.,3.89451831659521));
#17771=CARTESIAN_POINT('Origin',(136.021785697154,50.,3.89451831659521));
#17772=CARTESIAN_POINT('',(134.021785697154,48.,3.89451831659521));
#17773=CARTESIAN_POINT('Origin',(112.021785697154,48.,3.89451831659521));
#17774=CARTESIAN_POINT('',(110.021785697154,50.,3.89451831659521));
#17775=CARTESIAN_POINT('Origin',(112.021785697154,50.,3.89451831659521));
#17776=CARTESIAN_POINT('',(110.021785697154,48.,3.89451831659521));
#17777=CARTESIAN_POINT('Origin',(176.021785697154,48.,3.89451831659521));
#17778=CARTESIAN_POINT('',(174.021785697154,50.,3.89451831659521));
#17779=CARTESIAN_POINT('Origin',(176.021785697154,50.,3.89451831659521));
#17780=CARTESIAN_POINT('',(174.021785697154,48.,3.89451831659521));
#17781=CARTESIAN_POINT('Origin',(168.021785697154,48.,3.89451831659521));
#17782=CARTESIAN_POINT('',(166.021785697154,50.,3.89451831659521));
#17783=CARTESIAN_POINT('Origin',(168.021785697154,50.,3.89451831659521));
#17784=CARTESIAN_POINT('',(166.021785697154,48.,3.89451831659521));
#17785=CARTESIAN_POINT('Origin',(160.021785697154,48.,3.89451831659521));
#17786=CARTESIAN_POINT('',(158.021785697154,50.,3.89451831659521));
#17787=CARTESIAN_POINT('Origin',(160.021785697154,50.,3.89451831659521));
#17788=CARTESIAN_POINT('',(158.021785697154,48.,3.89451831659521));
#17789=CARTESIAN_POINT('Origin',(88.0217856971541,48.,3.89451831659521));
#17790=CARTESIAN_POINT('',(86.0217856971541,50.,3.89451831659521));
#17791=CARTESIAN_POINT('Origin',(88.0217856971541,50.,3.89451831659521));
#17792=CARTESIAN_POINT('',(86.0217856971541,48.,3.89451831659521));
#17793=CARTESIAN_POINT('Origin',(24.0217856971541,48.,3.89451831659521));
#17794=CARTESIAN_POINT('',(22.0217856971541,50.,3.89451831659521));
#17795=CARTESIAN_POINT('Origin',(24.0217856971541,50.,3.89451831659521));
#17796=CARTESIAN_POINT('',(22.0217856971541,48.,3.89451831659521));
#17797=CARTESIAN_POINT('Origin',(320.021785697154,48.,3.89451831659521));
#17798=CARTESIAN_POINT('',(318.021785697154,50.,3.89451831659521));
#17799=CARTESIAN_POINT('Origin',(320.021785697154,50.,3.89451831659521));
#17800=CARTESIAN_POINT('',(318.021785697154,48.,3.89451831659521));
#17801=CARTESIAN_POINT('Origin',(192.021785697154,48.,3.89451831659521));
#17802=CARTESIAN_POINT('',(190.021785697154,50.,3.89451831659521));
#17803=CARTESIAN_POINT('Origin',(192.021785697154,50.,3.89451831659521));
#17804=CARTESIAN_POINT('',(190.021785697154,48.,3.89451831659521));
#17805=CARTESIAN_POINT('Origin',(232.021785697154,48.,3.89451831659521));
#17806=CARTESIAN_POINT('',(230.021785697154,50.,3.89451831659521));
#17807=CARTESIAN_POINT('Origin',(232.021785697154,50.,3.89451831659521));
#17808=CARTESIAN_POINT('',(230.021785697154,48.,3.89451831659521));
#17809=CARTESIAN_POINT('Origin',(272.021785697154,48.,3.89451831659521));
#17810=CARTESIAN_POINT('',(270.021785697154,50.,3.89451831659521));
#17811=CARTESIAN_POINT('Origin',(272.021785697154,50.,3.89451831659521));
#17812=CARTESIAN_POINT('',(270.021785697154,48.,3.89451831659521));
#17813=CARTESIAN_POINT('Origin',(240.021785697154,48.,3.89451831659521));
#17814=CARTESIAN_POINT('',(238.021785697154,50.,3.89451831659521));
#17815=CARTESIAN_POINT('Origin',(240.021785697154,50.,3.89451831659521));
#17816=CARTESIAN_POINT('',(238.021785697154,48.,3.89451831659521));
#17817=CARTESIAN_POINT('Origin',(56.0217856971541,48.,3.89451831659521));
#17818=CARTESIAN_POINT('',(54.0217856971541,50.,3.89451831659521));
#17819=CARTESIAN_POINT('Origin',(56.0217856971541,50.,3.89451831659521));
#17820=CARTESIAN_POINT('',(54.0217856971541,48.,3.89451831659521));
#17821=CARTESIAN_POINT('Origin',(352.021785697154,48.,3.89451831659521));
#17822=CARTESIAN_POINT('',(350.021785697154,50.,3.89451831659521));
#17823=CARTESIAN_POINT('Origin',(352.021785697154,50.,3.89451831659521));
#17824=CARTESIAN_POINT('',(350.021785697154,48.,3.89451831659521));
#17825=CARTESIAN_POINT('Origin',(344.021785697154,48.,3.89451831659521));
#17826=CARTESIAN_POINT('',(342.021785697154,50.,3.89451831659521));
#17827=CARTESIAN_POINT('Origin',(344.021785697154,50.,3.89451831659521));
#17828=CARTESIAN_POINT('',(342.021785697154,48.,3.89451831659521));
#17829=CARTESIAN_POINT('Origin',(328.021785697154,48.,3.89451831659521));
#17830=CARTESIAN_POINT('',(326.021785697154,50.,3.89451831659521));
#17831=CARTESIAN_POINT('Origin',(328.021785697154,50.,3.89451831659521));
#17832=CARTESIAN_POINT('',(326.021785697154,48.,3.89451831659521));
#17833=CARTESIAN_POINT('Origin',(144.021785697154,48.,3.89451831659521));
#17834=CARTESIAN_POINT('',(142.021785697154,50.,3.89451831659521));
#17835=CARTESIAN_POINT('Origin',(144.021785697154,50.,3.89451831659521));
#17836=CARTESIAN_POINT('',(142.021785697154,48.,3.89451831659521));
#17837=CARTESIAN_POINT('Origin',(152.021785697154,48.,3.89451831659521));
#17838=CARTESIAN_POINT('',(150.021785697154,50.,3.89451831659521));
#17839=CARTESIAN_POINT('Origin',(152.021785697154,50.,3.89451831659521));
#17840=CARTESIAN_POINT('',(150.021785697154,48.,3.89451831659521));
#17841=CARTESIAN_POINT('Origin',(256.021785697154,48.,3.89451831659521));
#17842=CARTESIAN_POINT('',(254.021785697154,50.,3.89451831659521));
#17843=CARTESIAN_POINT('Origin',(256.021785697154,50.,3.89451831659521));
#17844=CARTESIAN_POINT('',(254.021785697154,48.,3.89451831659521));
#17845=CARTESIAN_POINT('Origin',(368.021785697154,48.,3.89451831659521));
#17846=CARTESIAN_POINT('',(366.021785697154,50.,3.89451831659521));
#17847=CARTESIAN_POINT('Origin',(368.021785697154,50.,3.89451831659521));
#17848=CARTESIAN_POINT('',(366.021785697154,48.,3.89451831659521));
#17849=CARTESIAN_POINT('Origin',(296.021785697154,48.,3.89451831659521));
#17850=CARTESIAN_POINT('',(294.021785697154,50.,3.89451831659521));
#17851=CARTESIAN_POINT('Origin',(296.021785697154,50.,3.89451831659521));
#17852=CARTESIAN_POINT('',(294.021785697154,48.,3.89451831659521));
#17853=CARTESIAN_POINT('Origin',(224.021785697154,48.,3.89451831659521));
#17854=CARTESIAN_POINT('',(222.021785697154,50.,3.89451831659521));
#17855=CARTESIAN_POINT('Origin',(224.021785697154,50.,3.89451831659521));
#17856=CARTESIAN_POINT('',(222.021785697154,48.,3.89451831659521));
#17857=CARTESIAN_POINT('Origin',(312.021785697154,48.,3.89451831659521));
#17858=CARTESIAN_POINT('',(310.021785697154,50.,3.89451831659521));
#17859=CARTESIAN_POINT('Origin',(312.021785697154,50.,3.89451831659521));
#17860=CARTESIAN_POINT('',(310.021785697154,48.,3.89451831659521));
#17861=CARTESIAN_POINT('Origin',(384.,48.,0.));
#17862=CARTESIAN_POINT('',(384.,50.,0.));
#17863=CARTESIAN_POINT('',(0.,50.,0.));
#17864=CARTESIAN_POINT('',(384.,48.,0.));
#17865=CARTESIAN_POINT('Origin',(192.,50.,11.));
#17866=CARTESIAN_POINT('',(384.,50.,12.));
#17867=CARTESIAN_POINT('Origin',(8.02178569715406,0.,3.89451831659521));
#17868=CARTESIAN_POINT('',(6.02178569715406,2.,3.89451831659521));
#17869=CARTESIAN_POINT('Origin',(8.02178569715406,2.,3.89451831659521));
#17870=CARTESIAN_POINT('',(6.02178569715406,0.,3.89451831659521));
#17871=CARTESIAN_POINT('',(6.02178569715406,0.,3.89451831659521));
#17872=CARTESIAN_POINT('Origin',(8.02178569715406,0.,3.89451831659521));
#17873=CARTESIAN_POINT('Origin',(304.021785697154,0.,3.89451831659521));
#17874=CARTESIAN_POINT('',(302.021785697154,2.,3.89451831659521));
#17875=CARTESIAN_POINT('Origin',(304.021785697154,2.,3.89451831659521));
#17876=CARTESIAN_POINT('',(302.021785697154,0.,3.89451831659521));
#17877=CARTESIAN_POINT('',(302.021785697154,0.,3.89451831659521));
#17878=CARTESIAN_POINT('Origin',(304.021785697154,0.,3.89451831659521));
#17879=CARTESIAN_POINT('Origin',(360.021785697154,0.,3.89451831659521));
#17880=CARTESIAN_POINT('',(358.021785697154,2.,3.89451831659521));
#17881=CARTESIAN_POINT('Origin',(360.021785697154,2.,3.89451831659521));
#17882=CARTESIAN_POINT('',(358.021785697154,0.,3.89451831659521));
#17883=CARTESIAN_POINT('',(358.021785697154,0.,3.89451831659521));
#17884=CARTESIAN_POINT('Origin',(360.021785697154,0.,3.89451831659521));
#17885=CARTESIAN_POINT('Origin',(208.021785697154,0.,3.89451831659521));
#17886=CARTESIAN_POINT('',(206.021785697154,2.,3.89451831659521));
#17887=CARTESIAN_POINT('Origin',(208.021785697154,2.,3.89451831659521));
#17888=CARTESIAN_POINT('',(206.021785697154,0.,3.89451831659521));
#17889=CARTESIAN_POINT('',(206.021785697154,0.,3.89451831659521));
#17890=CARTESIAN_POINT('Origin',(208.021785697154,0.,3.89451831659521));
#17891=CARTESIAN_POINT('Origin',(376.021785697154,0.,3.89451831659521));
#17892=CARTESIAN_POINT('',(374.021785697154,2.,3.89451831659521));
#17893=CARTESIAN_POINT('Origin',(376.021785697154,2.,3.89451831659521));
#17894=CARTESIAN_POINT('',(374.021785697154,0.,3.89451831659521));
#17895=CARTESIAN_POINT('',(374.021785697154,0.,3.89451831659521));
#17896=CARTESIAN_POINT('Origin',(376.021785697154,0.,3.89451831659521));
#17897=CARTESIAN_POINT('Origin',(16.0217856971541,0.,3.89451831659521));
#17898=CARTESIAN_POINT('',(14.0217856971541,2.,3.89451831659521));
#17899=CARTESIAN_POINT('Origin',(16.0217856971541,2.,3.89451831659521));
#17900=CARTESIAN_POINT('',(14.0217856971541,0.,3.89451831659521));
#17901=CARTESIAN_POINT('',(14.0217856971541,0.,3.89451831659521));
#17902=CARTESIAN_POINT('Origin',(16.0217856971541,0.,3.89451831659521));
#17903=CARTESIAN_POINT('Origin',(184.021785697154,0.,3.89451831659521));
#17904=CARTESIAN_POINT('',(182.021785697154,2.,3.89451831659521));
#17905=CARTESIAN_POINT('Origin',(184.021785697154,2.,3.89451831659521));
#17906=CARTESIAN_POINT('',(182.021785697154,0.,3.89451831659521));
#17907=CARTESIAN_POINT('',(182.021785697154,0.,3.89451831659521));
#17908=CARTESIAN_POINT('Origin',(184.021785697154,0.,3.89451831659521));
#17909=CARTESIAN_POINT('Origin',(120.021785697154,0.,3.89451831659521));
#17910=CARTESIAN_POINT('',(118.021785697154,2.,3.89451831659521));
#17911=CARTESIAN_POINT('Origin',(120.021785697154,2.,3.89451831659521));
#17912=CARTESIAN_POINT('',(118.021785697154,0.,3.89451831659521));
#17913=CARTESIAN_POINT('',(118.021785697154,0.,3.89451831659521));
#17914=CARTESIAN_POINT('Origin',(120.021785697154,0.,3.89451831659521));
#17915=CARTESIAN_POINT('Origin',(128.021785697154,0.,3.89451831659521));
#17916=CARTESIAN_POINT('',(126.021785697154,2.,3.89451831659521));
#17917=CARTESIAN_POINT('Origin',(128.021785697154,2.,3.89451831659521));
#17918=CARTESIAN_POINT('',(126.021785697154,0.,3.89451831659521));
#17919=CARTESIAN_POINT('',(126.021785697154,0.,3.89451831659521));
#17920=CARTESIAN_POINT('Origin',(128.021785697154,0.,3.89451831659521));
#17921=CARTESIAN_POINT('Origin',(280.021785697154,0.,3.89451831659521));
#17922=CARTESIAN_POINT('',(278.021785697154,2.,3.89451831659521));
#17923=CARTESIAN_POINT('Origin',(280.021785697154,2.,3.89451831659521));
#17924=CARTESIAN_POINT('',(278.021785697154,0.,3.89451831659521));
#17925=CARTESIAN_POINT('',(278.021785697154,0.,3.89451831659521));
#17926=CARTESIAN_POINT('Origin',(280.021785697154,0.,3.89451831659521));
#17927=CARTESIAN_POINT('Origin',(96.0217856971541,0.,3.89451831659521));
#17928=CARTESIAN_POINT('',(94.0217856971541,2.,3.89451831659521));
#17929=CARTESIAN_POINT('Origin',(96.0217856971541,2.,3.89451831659521));
#17930=CARTESIAN_POINT('',(94.0217856971541,0.,3.89451831659521));
#17931=CARTESIAN_POINT('',(94.0217856971541,0.,3.89451831659521));
#17932=CARTESIAN_POINT('Origin',(96.0217856971541,0.,3.89451831659521));
#17933=CARTESIAN_POINT('Origin',(200.021785697154,0.,3.89451831659521));
#17934=CARTESIAN_POINT('',(198.021785697154,2.,3.89451831659521));
#17935=CARTESIAN_POINT('Origin',(200.021785697154,2.,3.89451831659521));
#17936=CARTESIAN_POINT('',(198.021785697154,0.,3.89451831659521));
#17937=CARTESIAN_POINT('',(198.021785697154,0.,3.89451831659521));
#17938=CARTESIAN_POINT('Origin',(200.021785697154,0.,3.89451831659521));
#17939=CARTESIAN_POINT('Origin',(72.0217856971541,0.,3.89451831659521));
#17940=CARTESIAN_POINT('',(70.0217856971541,2.,3.89451831659521));
#17941=CARTESIAN_POINT('Origin',(72.0217856971541,2.,3.89451831659521));
#17942=CARTESIAN_POINT('',(70.0217856971541,0.,3.89451831659521));
#17943=CARTESIAN_POINT('',(70.0217856971541,0.,3.89451831659521));
#17944=CARTESIAN_POINT('Origin',(72.0217856971541,0.,3.89451831659521));
#17945=CARTESIAN_POINT('Origin',(216.021785697154,0.,3.89451831659521));
#17946=CARTESIAN_POINT('',(214.021785697154,2.,3.89451831659521));
#17947=CARTESIAN_POINT('Origin',(216.021785697154,2.,3.89451831659521));
#17948=CARTESIAN_POINT('',(214.021785697154,0.,3.89451831659521));
#17949=CARTESIAN_POINT('',(214.021785697154,0.,3.89451831659521));
#17950=CARTESIAN_POINT('Origin',(216.021785697154,0.,3.89451831659521));
#17951=CARTESIAN_POINT('Origin',(248.021785697154,0.,3.89451831659521));
#17952=CARTESIAN_POINT('',(246.021785697154,2.,3.89451831659521));
#17953=CARTESIAN_POINT('Origin',(248.021785697154,2.,3.89451831659521));
#17954=CARTESIAN_POINT('',(246.021785697154,0.,3.89451831659521));
#17955=CARTESIAN_POINT('',(246.021785697154,0.,3.89451831659521));
#17956=CARTESIAN_POINT('Origin',(248.021785697154,0.,3.89451831659521));
#17957=CARTESIAN_POINT('Origin',(80.0217856971541,0.,3.89451831659521));
#17958=CARTESIAN_POINT('',(78.0217856971541,2.,3.89451831659521));
#17959=CARTESIAN_POINT('Origin',(80.0217856971541,2.,3.89451831659521));
#17960=CARTESIAN_POINT('',(78.0217856971541,0.,3.89451831659521));
#17961=CARTESIAN_POINT('',(78.0217856971541,0.,3.89451831659521));
#17962=CARTESIAN_POINT('Origin',(80.0217856971541,0.,3.89451831659521));
#17963=CARTESIAN_POINT('Origin',(264.021785697154,0.,3.89451831659521));
#17964=CARTESIAN_POINT('',(262.021785697154,2.,3.89451831659521));
#17965=CARTESIAN_POINT('Origin',(264.021785697154,2.,3.89451831659521));
#17966=CARTESIAN_POINT('',(262.021785697154,0.,3.89451831659521));
#17967=CARTESIAN_POINT('',(262.021785697154,0.,3.89451831659521));
#17968=CARTESIAN_POINT('Origin',(264.021785697154,0.,3.89451831659521));
#17969=CARTESIAN_POINT('Origin',(48.0217856971541,0.,3.89451831659521));
#17970=CARTESIAN_POINT('',(46.0217856971541,2.,3.89451831659521));
#17971=CARTESIAN_POINT('Origin',(48.0217856971541,2.,3.89451831659521));
#17972=CARTESIAN_POINT('',(46.0217856971541,0.,3.89451831659521));
#17973=CARTESIAN_POINT('',(46.0217856971541,0.,3.89451831659521));
#17974=CARTESIAN_POINT('Origin',(48.0217856971541,0.,3.89451831659521));
#17975=CARTESIAN_POINT('Origin',(32.0217856971541,0.,3.89451831659521));
#17976=CARTESIAN_POINT('',(30.0217856971541,2.,3.89451831659521));
#17977=CARTESIAN_POINT('Origin',(32.0217856971541,2.,3.89451831659521));
#17978=CARTESIAN_POINT('',(30.0217856971541,0.,3.89451831659521));
#17979=CARTESIAN_POINT('',(30.0217856971541,0.,3.89451831659521));
#17980=CARTESIAN_POINT('Origin',(32.0217856971541,0.,3.89451831659521));
#17981=CARTESIAN_POINT('Origin',(336.021785697154,0.,3.89451831659521));
#17982=CARTESIAN_POINT('',(334.021785697154,2.,3.89451831659521));
#17983=CARTESIAN_POINT('Origin',(336.021785697154,2.,3.89451831659521));
#17984=CARTESIAN_POINT('',(334.021785697154,0.,3.89451831659521));
#17985=CARTESIAN_POINT('',(334.021785697154,0.,3.89451831659521));
#17986=CARTESIAN_POINT('Origin',(336.021785697154,0.,3.89451831659521));
#17987=CARTESIAN_POINT('Origin',(40.0217856971541,0.,3.89451831659521));
#17988=CARTESIAN_POINT('',(38.0217856971541,2.,3.89451831659521));
#17989=CARTESIAN_POINT('Origin',(40.0217856971541,2.,3.89451831659521));
#17990=CARTESIAN_POINT('',(38.0217856971541,0.,3.89451831659521));
#17991=CARTESIAN_POINT('',(38.0217856971541,0.,3.89451831659521));
#17992=CARTESIAN_POINT('Origin',(40.0217856971541,0.,3.89451831659521));
#17993=CARTESIAN_POINT('Origin',(104.021785697154,0.,3.89451831659521));
#17994=CARTESIAN_POINT('',(102.021785697154,2.,3.89451831659521));
#17995=CARTESIAN_POINT('Origin',(104.021785697154,2.,3.89451831659521));
#17996=CARTESIAN_POINT('',(102.021785697154,0.,3.89451831659521));
#17997=CARTESIAN_POINT('',(102.021785697154,0.,3.89451831659521));
#17998=CARTESIAN_POINT('Origin',(104.021785697154,0.,3.89451831659521));
#17999=CARTESIAN_POINT('Origin',(64.0217856971541,0.,3.89451831659521));
#18000=CARTESIAN_POINT('',(62.0217856971541,2.,3.89451831659521));
#18001=CARTESIAN_POINT('Origin',(64.0217856971541,2.,3.89451831659521));
#18002=CARTESIAN_POINT('',(62.0217856971541,0.,3.89451831659521));
#18003=CARTESIAN_POINT('',(62.0217856971541,0.,3.89451831659521));
#18004=CARTESIAN_POINT('Origin',(64.0217856971541,0.,3.89451831659521));
#18005=CARTESIAN_POINT('Origin',(288.021785697154,0.,3.89451831659521));
#18006=CARTESIAN_POINT('',(286.021785697154,2.,3.89451831659521));
#18007=CARTESIAN_POINT('Origin',(288.021785697154,2.,3.89451831659521));
#18008=CARTESIAN_POINT('',(286.021785697154,0.,3.89451831659521));
#18009=CARTESIAN_POINT('',(286.021785697154,0.,3.89451831659521));
#18010=CARTESIAN_POINT('Origin',(288.021785697154,0.,3.89451831659521));
#18011=CARTESIAN_POINT('Origin',(136.021785697154,0.,3.89451831659521));
#18012=CARTESIAN_POINT('',(134.021785697154,2.,3.89451831659521));
#18013=CARTESIAN_POINT('Origin',(136.021785697154,2.,3.89451831659521));
#18014=CARTESIAN_POINT('',(134.021785697154,0.,3.89451831659521));
#18015=CARTESIAN_POINT('',(134.021785697154,0.,3.89451831659521));
#18016=CARTESIAN_POINT('Origin',(136.021785697154,0.,3.89451831659521));
#18017=CARTESIAN_POINT('Origin',(112.021785697154,0.,3.89451831659521));
#18018=CARTESIAN_POINT('',(110.021785697154,2.,3.89451831659521));
#18019=CARTESIAN_POINT('Origin',(112.021785697154,2.,3.89451831659521));
#18020=CARTESIAN_POINT('',(110.021785697154,0.,3.89451831659521));
#18021=CARTESIAN_POINT('',(110.021785697154,0.,3.89451831659521));
#18022=CARTESIAN_POINT('Origin',(112.021785697154,0.,3.89451831659521));
#18023=CARTESIAN_POINT('Origin',(176.021785697154,0.,3.89451831659521));
#18024=CARTESIAN_POINT('',(174.021785697154,2.,3.89451831659521));
#18025=CARTESIAN_POINT('Origin',(176.021785697154,2.,3.89451831659521));
#18026=CARTESIAN_POINT('',(174.021785697154,0.,3.89451831659521));
#18027=CARTESIAN_POINT('',(174.021785697154,0.,3.89451831659521));
#18028=CARTESIAN_POINT('Origin',(176.021785697154,0.,3.89451831659521));
#18029=CARTESIAN_POINT('Origin',(168.021785697154,0.,3.89451831659521));
#18030=CARTESIAN_POINT('',(166.021785697154,2.,3.89451831659521));
#18031=CARTESIAN_POINT('Origin',(168.021785697154,2.,3.89451831659521));
#18032=CARTESIAN_POINT('',(166.021785697154,0.,3.89451831659521));
#18033=CARTESIAN_POINT('',(166.021785697154,0.,3.89451831659521));
#18034=CARTESIAN_POINT('Origin',(168.021785697154,0.,3.89451831659521));
#18035=CARTESIAN_POINT('Origin',(160.021785697154,0.,3.89451831659521));
#18036=CARTESIAN_POINT('',(158.021785697154,2.,3.89451831659521));
#18037=CARTESIAN_POINT('Origin',(160.021785697154,2.,3.89451831659521));
#18038=CARTESIAN_POINT('',(158.021785697154,0.,3.89451831659521));
#18039=CARTESIAN_POINT('',(158.021785697154,0.,3.89451831659521));
#18040=CARTESIAN_POINT('Origin',(160.021785697154,0.,3.89451831659521));
#18041=CARTESIAN_POINT('Origin',(88.0217856971541,0.,3.89451831659521));
#18042=CARTESIAN_POINT('',(86.0217856971541,2.,3.89451831659521));
#18043=CARTESIAN_POINT('Origin',(88.0217856971541,2.,3.89451831659521));
#18044=CARTESIAN_POINT('',(86.0217856971541,0.,3.89451831659521));
#18045=CARTESIAN_POINT('',(86.0217856971541,0.,3.89451831659521));
#18046=CARTESIAN_POINT('Origin',(88.0217856971541,0.,3.89451831659521));
#18047=CARTESIAN_POINT('Origin',(24.0217856971541,0.,3.89451831659521));
#18048=CARTESIAN_POINT('',(22.0217856971541,2.,3.89451831659521));
#18049=CARTESIAN_POINT('Origin',(24.0217856971541,2.,3.89451831659521));
#18050=CARTESIAN_POINT('',(22.0217856971541,0.,3.89451831659521));
#18051=CARTESIAN_POINT('',(22.0217856971541,0.,3.89451831659521));
#18052=CARTESIAN_POINT('Origin',(24.0217856971541,0.,3.89451831659521));
#18053=CARTESIAN_POINT('Origin',(320.021785697154,0.,3.89451831659521));
#18054=CARTESIAN_POINT('',(318.021785697154,2.,3.89451831659521));
#18055=CARTESIAN_POINT('Origin',(320.021785697154,2.,3.89451831659521));
#18056=CARTESIAN_POINT('',(318.021785697154,0.,3.89451831659521));
#18057=CARTESIAN_POINT('',(318.021785697154,0.,3.89451831659521));
#18058=CARTESIAN_POINT('Origin',(320.021785697154,0.,3.89451831659521));
#18059=CARTESIAN_POINT('Origin',(192.021785697154,0.,3.89451831659521));
#18060=CARTESIAN_POINT('',(190.021785697154,2.,3.89451831659521));
#18061=CARTESIAN_POINT('Origin',(192.021785697154,2.,3.89451831659521));
#18062=CARTESIAN_POINT('',(190.021785697154,0.,3.89451831659521));
#18063=CARTESIAN_POINT('',(190.021785697154,0.,3.89451831659521));
#18064=CARTESIAN_POINT('Origin',(192.021785697154,0.,3.89451831659521));
#18065=CARTESIAN_POINT('Origin',(232.021785697154,0.,3.89451831659521));
#18066=CARTESIAN_POINT('',(230.021785697154,2.,3.89451831659521));
#18067=CARTESIAN_POINT('Origin',(232.021785697154,2.,3.89451831659521));
#18068=CARTESIAN_POINT('',(230.021785697154,0.,3.89451831659521));
#18069=CARTESIAN_POINT('',(230.021785697154,0.,3.89451831659521));
#18070=CARTESIAN_POINT('Origin',(232.021785697154,0.,3.89451831659521));
#18071=CARTESIAN_POINT('Origin',(272.021785697154,0.,3.89451831659521));
#18072=CARTESIAN_POINT('',(270.021785697154,2.,3.89451831659521));
#18073=CARTESIAN_POINT('Origin',(272.021785697154,2.,3.89451831659521));
#18074=CARTESIAN_POINT('',(270.021785697154,0.,3.89451831659521));
#18075=CARTESIAN_POINT('',(270.021785697154,0.,3.89451831659521));
#18076=CARTESIAN_POINT('Origin',(272.021785697154,0.,3.89451831659521));
#18077=CARTESIAN_POINT('Origin',(240.021785697154,0.,3.89451831659521));
#18078=CARTESIAN_POINT('',(238.021785697154,2.,3.89451831659521));
#18079=CARTESIAN_POINT('Origin',(240.021785697154,2.,3.89451831659521));
#18080=CARTESIAN_POINT('',(238.021785697154,0.,3.89451831659521));
#18081=CARTESIAN_POINT('',(238.021785697154,0.,3.89451831659521));
#18082=CARTESIAN_POINT('Origin',(240.021785697154,0.,3.89451831659521));
#18083=CARTESIAN_POINT('Origin',(56.0217856971541,0.,3.89451831659521));
#18084=CARTESIAN_POINT('',(54.0217856971541,2.,3.89451831659521));
#18085=CARTESIAN_POINT('Origin',(56.0217856971541,2.,3.89451831659521));
#18086=CARTESIAN_POINT('',(54.0217856971541,0.,3.89451831659521));
#18087=CARTESIAN_POINT('',(54.0217856971541,0.,3.89451831659521));
#18088=CARTESIAN_POINT('Origin',(56.0217856971541,0.,3.89451831659521));
#18089=CARTESIAN_POINT('Origin',(352.021785697154,0.,3.89451831659521));
#18090=CARTESIAN_POINT('',(350.021785697154,2.,3.89451831659521));
#18091=CARTESIAN_POINT('Origin',(352.021785697154,2.,3.89451831659521));
#18092=CARTESIAN_POINT('',(350.021785697154,0.,3.89451831659521));
#18093=CARTESIAN_POINT('',(350.021785697154,0.,3.89451831659521));
#18094=CARTESIAN_POINT('Origin',(352.021785697154,0.,3.89451831659521));
#18095=CARTESIAN_POINT('Origin',(344.021785697154,0.,3.89451831659521));
#18096=CARTESIAN_POINT('',(342.021785697154,2.,3.89451831659521));
#18097=CARTESIAN_POINT('Origin',(344.021785697154,2.,3.89451831659521));
#18098=CARTESIAN_POINT('',(342.021785697154,0.,3.89451831659521));
#18099=CARTESIAN_POINT('',(342.021785697154,0.,3.89451831659521));
#18100=CARTESIAN_POINT('Origin',(344.021785697154,0.,3.89451831659521));
#18101=CARTESIAN_POINT('Origin',(328.021785697154,0.,3.89451831659521));
#18102=CARTESIAN_POINT('',(326.021785697154,2.,3.89451831659521));
#18103=CARTESIAN_POINT('Origin',(328.021785697154,2.,3.89451831659521));
#18104=CARTESIAN_POINT('',(326.021785697154,0.,3.89451831659521));
#18105=CARTESIAN_POINT('',(326.021785697154,0.,3.89451831659521));
#18106=CARTESIAN_POINT('Origin',(328.021785697154,0.,3.89451831659521));
#18107=CARTESIAN_POINT('Origin',(144.021785697154,0.,3.89451831659521));
#18108=CARTESIAN_POINT('',(142.021785697154,2.,3.89451831659521));
#18109=CARTESIAN_POINT('Origin',(144.021785697154,2.,3.89451831659521));
#18110=CARTESIAN_POINT('',(142.021785697154,0.,3.89451831659521));
#18111=CARTESIAN_POINT('',(142.021785697154,0.,3.89451831659521));
#18112=CARTESIAN_POINT('Origin',(144.021785697154,0.,3.89451831659521));
#18113=CARTESIAN_POINT('Origin',(152.021785697154,0.,3.89451831659521));
#18114=CARTESIAN_POINT('',(150.021785697154,2.,3.89451831659521));
#18115=CARTESIAN_POINT('Origin',(152.021785697154,2.,3.89451831659521));
#18116=CARTESIAN_POINT('',(150.021785697154,0.,3.89451831659521));
#18117=CARTESIAN_POINT('',(150.021785697154,0.,3.89451831659521));
#18118=CARTESIAN_POINT('Origin',(152.021785697154,0.,3.89451831659521));
#18119=CARTESIAN_POINT('Origin',(256.021785697154,0.,3.89451831659521));
#18120=CARTESIAN_POINT('',(254.021785697154,2.,3.89451831659521));
#18121=CARTESIAN_POINT('Origin',(256.021785697154,2.,3.89451831659521));
#18122=CARTESIAN_POINT('',(254.021785697154,0.,3.89451831659521));
#18123=CARTESIAN_POINT('',(254.021785697154,0.,3.89451831659521));
#18124=CARTESIAN_POINT('Origin',(256.021785697154,0.,3.89451831659521));
#18125=CARTESIAN_POINT('Origin',(368.021785697154,0.,3.89451831659521));
#18126=CARTESIAN_POINT('',(366.021785697154,2.,3.89451831659521));
#18127=CARTESIAN_POINT('Origin',(368.021785697154,2.,3.89451831659521));
#18128=CARTESIAN_POINT('',(366.021785697154,0.,3.89451831659521));
#18129=CARTESIAN_POINT('',(366.021785697154,0.,3.89451831659521));
#18130=CARTESIAN_POINT('Origin',(368.021785697154,0.,3.89451831659521));
#18131=CARTESIAN_POINT('Origin',(296.021785697154,0.,3.89451831659521));
#18132=CARTESIAN_POINT('',(294.021785697154,2.,3.89451831659521));
#18133=CARTESIAN_POINT('Origin',(296.021785697154,2.,3.89451831659521));
#18134=CARTESIAN_POINT('',(294.021785697154,0.,3.89451831659521));
#18135=CARTESIAN_POINT('',(294.021785697154,0.,3.89451831659521));
#18136=CARTESIAN_POINT('Origin',(296.021785697154,0.,3.89451831659521));
#18137=CARTESIAN_POINT('Origin',(224.021785697154,0.,3.89451831659521));
#18138=CARTESIAN_POINT('',(222.021785697154,2.,3.89451831659521));
#18139=CARTESIAN_POINT('Origin',(224.021785697154,2.,3.89451831659521));
#18140=CARTESIAN_POINT('',(222.021785697154,0.,3.89451831659521));
#18141=CARTESIAN_POINT('',(222.021785697154,0.,3.89451831659521));
#18142=CARTESIAN_POINT('Origin',(224.021785697154,0.,3.89451831659521));
#18143=CARTESIAN_POINT('Origin',(312.021785697154,0.,3.89451831659521));
#18144=CARTESIAN_POINT('',(310.021785697154,2.,3.89451831659521));
#18145=CARTESIAN_POINT('Origin',(312.021785697154,2.,3.89451831659521));
#18146=CARTESIAN_POINT('',(310.021785697154,0.,3.89451831659521));
#18147=CARTESIAN_POINT('',(310.021785697154,0.,3.89451831659521));
#18148=CARTESIAN_POINT('Origin',(312.021785697154,0.,3.89451831659521));
#18149=CARTESIAN_POINT('Origin',(384.,0.,0.));
#18150=CARTESIAN_POINT('',(384.,0.,0.));
#18151=CARTESIAN_POINT('',(0.,0.,0.));
#18152=CARTESIAN_POINT('',(384.,2.,0.));
#18153=CARTESIAN_POINT('',(0.,2.,0.));
#18154=CARTESIAN_POINT('',(384.,0.,0.));
#18155=CARTESIAN_POINT('Origin',(384.,0.,10.));
#18156=CARTESIAN_POINT('',(384.,0.,0.));
#18157=CARTESIAN_POINT('',(384.,2.,0.));
#18158=CARTESIAN_POINT('Origin',(192.,2.,5.));
#18159=CARTESIAN_POINT('Origin',(192.,0.,5.));
#18160=CARTESIAN_POINT('',(0.,0.,0.));
#18161=CARTESIAN_POINT('Origin',(363.987734179926,50.,25.7372649179816));
#18162=CARTESIAN_POINT('',(362.487734179926,50.,25.7372649179816));
#18163=CARTESIAN_POINT('Origin',(363.987734179926,50.,25.7372649179816));
#18164=CARTESIAN_POINT('',(362.487734179926,53.,25.7372649179816));
#18165=CARTESIAN_POINT('',(362.487734179926,50.,25.7372649179816));
#18166=CARTESIAN_POINT('Origin',(363.987734179926,53.,25.7372649179816));
#18167=CARTESIAN_POINT('Origin',(368.021785697154,53.,3.89451831659521));
#18168=CARTESIAN_POINT('',(370.021785697154,53.,3.89451831659521));
#18169=CARTESIAN_POINT('Origin',(368.021785697154,53.,3.89451831659521));
#18170=CARTESIAN_POINT('',(370.021785697154,50.,3.89451831659521));
#18171=CARTESIAN_POINT('',(370.021785697154,53.,3.89451831659521));
#18172=CARTESIAN_POINT('Origin',(368.021785697154,50.,3.89451831659521));
#18173=CARTESIAN_POINT('Origin',(360.021785697154,53.,3.89451831659521));
#18174=CARTESIAN_POINT('',(362.021785697154,53.,3.89451831659521));
#18175=CARTESIAN_POINT('Origin',(360.021785697154,53.,3.89451831659521));
#18176=CARTESIAN_POINT('',(362.021785697154,50.,3.89451831659521));
#18177=CARTESIAN_POINT('',(362.021785697154,53.,3.89451831659521));
#18178=CARTESIAN_POINT('Origin',(360.021785697154,50.,3.89451831659521));
#18179=CARTESIAN_POINT('Origin',(367.952200273994,48.,28.4747649179816));
#18180=CARTESIAN_POINT('',(371.916666368061,50.,28.4747649179816));
#18181=CARTESIAN_POINT('',(371.916666368061,48.,30.4747649179816));
#18182=CARTESIAN_POINT('Origin',(371.916666368061,48.,28.4747649179816));
#18183=CARTESIAN_POINT('',(356.058801991792,48.,30.4747649179816));
#18184=CARTESIAN_POINT('',(367.952200273994,48.,30.4747649179816));
#18185=CARTESIAN_POINT('',(356.058801991792,50.,28.4747649179816));
#18186=CARTESIAN_POINT('Origin',(356.058801991792,48.,28.4747649179816));
#18187=CARTESIAN_POINT('',(367.952200273994,50.,28.4747649179816));
#18188=CARTESIAN_POINT('Origin',(363.987734179926,35.4644660940673,30.4747649179816));
#18189=CARTESIAN_POINT('',(371.916666368061,32.0710678118655,30.4747649179816));
#18190=CARTESIAN_POINT('',(371.916666368061,50.,30.4747649179816));
#18191=CARTESIAN_POINT('',(378.987734179926,25.,30.4747649179816));
#18192=CARTESIAN_POINT('',(378.987734179926,25.,30.4747649179816));
#18193=CARTESIAN_POINT('',(371.916666368061,17.9289321881345,30.4747649179816));
#18194=CARTESIAN_POINT('',(378.987734179926,25.,30.4747649179816));
#18195=CARTESIAN_POINT('',(356.058801991792,17.9289321881345,30.4747649179816));
#18196=CARTESIAN_POINT('',(371.916666368061,17.9289321881345,30.4747649179816));
#18197=CARTESIAN_POINT('',(348.987734179926,25.,30.4747649179816));
#18198=CARTESIAN_POINT('',(348.987734179926,25.,30.4747649179816));
#18199=CARTESIAN_POINT('',(356.058801991792,32.0710678118655,30.4747649179816));
#18200=CARTESIAN_POINT('',(348.987734179926,25.,30.4747649179816));
#18201=CARTESIAN_POINT('',(356.058801991792,50.,30.4747649179816));
#18202=CARTESIAN_POINT('',(362.381415464215,29.,30.4747649179816));
#18203=CARTESIAN_POINT('Origin',(363.881415464215,29.,30.4747649179816));
#18204=CARTESIAN_POINT('',(353.131415464215,25.,30.4747649179816));
#18205=CARTESIAN_POINT('Origin',(354.631415464215,25.,30.4747649179816));
#18206=CARTESIAN_POINT('',(367.006415464215,21.,30.4747649179816));
#18207=CARTESIAN_POINT('Origin',(368.506415464215,21.,30.4747649179816));
#18208=CARTESIAN_POINT('',(357.756415464215,21.,30.4747649179816));
#18209=CARTESIAN_POINT('Origin',(359.256415464215,21.,30.4747649179816));
#18210=CARTESIAN_POINT('',(362.381415464215,25.,30.4747649179816));
#18211=CARTESIAN_POINT('Origin',(363.881415464215,25.,30.4747649179816));
#18212=CARTESIAN_POINT('',(362.381415464215,21.,30.4747649179816));
#18213=CARTESIAN_POINT('Origin',(363.881415464215,21.,30.4747649179816));
#18214=CARTESIAN_POINT('',(367.006415464215,25.,30.4747649179816));
#18215=CARTESIAN_POINT('Origin',(368.506415464215,25.,30.4747649179816));
#18216=CARTESIAN_POINT('',(357.756415464215,25.,30.4747649179816));
#18217=CARTESIAN_POINT('Origin',(359.256415464215,25.,30.4747649179816));
#18218=CARTESIAN_POINT('',(357.756415464215,29.,30.4747649179816));
#18219=CARTESIAN_POINT('Origin',(359.256415464215,29.,30.4747649179816));
#18220=CARTESIAN_POINT('',(367.006415464215,29.,30.4747649179816));
#18221=CARTESIAN_POINT('Origin',(368.506415464215,29.,30.4747649179816));
#18222=CARTESIAN_POINT('',(371.631415464215,25.,30.4747649179816));
#18223=CARTESIAN_POINT('Origin',(373.131415464215,25.,30.4747649179816));
#18224=CARTESIAN_POINT('Origin',(356.058801991792,49.0313730334031,29.9747649179816));
#18225=CARTESIAN_POINT('',(356.058801991792,53.,30.4747649179816));
#18226=CARTESIAN_POINT('',(356.058801991792,49.0313730334031,33.9747649179816));
#18227=CARTESIAN_POINT('Origin',(356.058801991792,49.0313730334031,29.9747649179816));
#18228=CARTESIAN_POINT('',(371.916666368061,49.0313730334031,33.9747649179816));
#18229=CARTESIAN_POINT('',(356.058801991792,49.0313730334031,33.9747649179816));
#18230=CARTESIAN_POINT('',(371.916666368061,53.,30.4747649179816));
#18231=CARTESIAN_POINT('Origin',(371.916666368061,49.0313730334031,29.9747649179816));
#18232=CARTESIAN_POINT('',(356.058801991792,53.,30.4747649179816));
#18233=CARTESIAN_POINT('Origin',(363.987734179926,35.4644660940673,33.9747649179816));
#18234=CARTESIAN_POINT('',(356.058801991792,32.0710678118655,33.9747649179816));
#18235=CARTESIAN_POINT('',(356.058801991792,50.,33.9747649179816));
#18236=CARTESIAN_POINT('',(348.987734179926,25.,33.9747649179816));
#18237=CARTESIAN_POINT('',(348.987734179926,25.,33.9747649179816));
#18238=CARTESIAN_POINT('',(356.058801991792,17.9289321881345,33.9747649179816));
#18239=CARTESIAN_POINT('',(348.987734179926,25.,33.9747649179816));
#18240=CARTESIAN_POINT('',(371.916666368061,17.9289321881345,33.9747649179816));
#18241=CARTESIAN_POINT('',(371.916666368061,17.9289321881345,33.9747649179816));
#18242=CARTESIAN_POINT('',(378.987734179926,25.,33.9747649179816));
#18243=CARTESIAN_POINT('',(378.987734179926,25.,33.9747649179816));
#18244=CARTESIAN_POINT('',(371.916666368061,32.0710678118655,33.9747649179816));
#18245=CARTESIAN_POINT('',(378.987734179926,25.,33.9747649179816));
#18246=CARTESIAN_POINT('',(371.916666368061,50.,33.9747649179816));
#18247=CARTESIAN_POINT('',(371.631415464215,25.,33.9747649179816));
#18248=CARTESIAN_POINT('Origin',(373.131415464215,25.,33.9747649179816));
#18249=CARTESIAN_POINT('',(367.006415464215,29.,33.9747649179816));
#18250=CARTESIAN_POINT('Origin',(368.506415464215,29.,33.9747649179816));
#18251=CARTESIAN_POINT('',(357.756415464215,29.,33.9747649179816));
#18252=CARTESIAN_POINT('Origin',(359.256415464215,29.,33.9747649179816));
#18253=CARTESIAN_POINT('',(357.756415464215,25.,33.9747649179816));
#18254=CARTESIAN_POINT('Origin',(359.256415464215,25.,33.9747649179816));
#18255=CARTESIAN_POINT('',(367.006415464215,25.,33.9747649179816));
#18256=CARTESIAN_POINT('Origin',(368.506415464215,25.,33.9747649179816));
#18257=CARTESIAN_POINT('',(362.381415464215,21.,33.9747649179816));
#18258=CARTESIAN_POINT('Origin',(363.881415464215,21.,33.9747649179816));
#18259=CARTESIAN_POINT('',(362.381415464215,25.,33.9747649179816));
#18260=CARTESIAN_POINT('Origin',(363.881415464215,25.,33.9747649179816));
#18261=CARTESIAN_POINT('',(357.756415464215,21.,33.9747649179816));
#18262=CARTESIAN_POINT('Origin',(359.256415464215,21.,33.9747649179816));
#18263=CARTESIAN_POINT('',(367.006415464215,21.,33.9747649179816));
#18264=CARTESIAN_POINT('Origin',(368.506415464215,21.,33.9747649179816));
#18265=CARTESIAN_POINT('',(353.131415464215,25.,33.9747649179816));
#18266=CARTESIAN_POINT('Origin',(354.631415464215,25.,33.9747649179816));
#18267=CARTESIAN_POINT('',(362.381415464215,29.,33.9747649179816));
#18268=CARTESIAN_POINT('Origin',(363.881415464215,29.,33.9747649179816));
#18269=CARTESIAN_POINT('Origin',(373.131415464215,25.,30.4747649179816));
#18270=CARTESIAN_POINT('',(371.631415464215,25.,30.4747649179816));
#18271=CARTESIAN_POINT('Origin',(368.506415464215,29.,30.4747649179816));
#18272=CARTESIAN_POINT('',(367.006415464215,29.,30.4747649179816));
#18273=CARTESIAN_POINT('Origin',(359.256415464215,29.,30.4747649179816));
#18274=CARTESIAN_POINT('',(357.756415464215,29.,30.4747649179816));
#18275=CARTESIAN_POINT('Origin',(359.256415464215,25.,30.4747649179816));
#18276=CARTESIAN_POINT('',(357.756415464215,25.,30.4747649179816));
#18277=CARTESIAN_POINT('Origin',(368.506415464215,25.,30.4747649179816));
#18278=CARTESIAN_POINT('',(367.006415464215,25.,30.4747649179816));
#18279=CARTESIAN_POINT('Origin',(363.881415464215,21.,30.4747649179816));
#18280=CARTESIAN_POINT('',(362.381415464215,21.,30.4747649179816));
#18281=CARTESIAN_POINT('Origin',(363.881415464215,25.,30.4747649179816));
#18282=CARTESIAN_POINT('',(362.381415464215,25.,30.4747649179816));
#18283=CARTESIAN_POINT('Origin',(359.256415464215,21.,30.4747649179816));
#18284=CARTESIAN_POINT('',(357.756415464215,21.,30.4747649179816));
#18285=CARTESIAN_POINT('Origin',(368.506415464215,21.,30.4747649179816));
#18286=CARTESIAN_POINT('',(367.006415464215,21.,30.4747649179816));
#18287=CARTESIAN_POINT('Origin',(354.631415464215,25.,30.4747649179816));
#18288=CARTESIAN_POINT('',(353.131415464215,25.,30.4747649179816));
#18289=CARTESIAN_POINT('Origin',(363.881415464215,29.,30.4747649179816));
#18290=CARTESIAN_POINT('',(362.381415464215,29.,30.4747649179816));
#18291=CARTESIAN_POINT('Origin',(356.058801991792,32.0710678118655,30.4747649179816));
#18292=CARTESIAN_POINT('',(348.987734179926,25.,30.4747649179816));
#18293=CARTESIAN_POINT('',(356.058801991792,32.0710678118655,30.4747649179816));
#18294=CARTESIAN_POINT('Origin',(378.987734179926,25.,30.4747649179816));
#18295=CARTESIAN_POINT('',(371.916666368061,32.0710678118655,30.4747649179816));
#18296=CARTESIAN_POINT('',(378.987734179926,25.,30.4747649179816));
#18297=CARTESIAN_POINT('Origin',(371.916666368061,17.9289321881345,30.4747649179816));
#18298=CARTESIAN_POINT('',(371.916666368061,17.9289321881345,30.4747649179816));
#18299=CARTESIAN_POINT('Origin',(356.058801991792,17.9289321881345,30.4747649179816));
#18300=CARTESIAN_POINT('',(356.058801991792,17.9289321881345,30.4747649179816));
#18301=CARTESIAN_POINT('Origin',(348.987734179926,25.,30.4747649179816));
#18302=CARTESIAN_POINT('Origin',(363.987734179926,35.4644660940673,19.4747649179816));
#18303=CARTESIAN_POINT('',(371.916666368061,50.,19.4747649179816));
#18304=CARTESIAN_POINT('',(356.058801991792,50.,19.4747649179816));
#18305=CARTESIAN_POINT('',(367.952200273994,50.,19.4747649179816));
#18306=CARTESIAN_POINT('',(371.916666368061,32.0710678118655,19.4747649179816));
#18307=CARTESIAN_POINT('',(371.916666368061,50.,19.4747649179816));
#18308=CARTESIAN_POINT('',(378.987734179926,25.,19.4747649179816));
#18309=CARTESIAN_POINT('',(378.987734179926,25.,19.4747649179816));
#18310=CARTESIAN_POINT('',(371.916666368061,17.9289321881345,19.4747649179816));
#18311=CARTESIAN_POINT('',(378.987734179926,25.,19.4747649179816));
#18312=CARTESIAN_POINT('',(356.058801991792,17.9289321881345,19.4747649179816));
#18313=CARTESIAN_POINT('',(371.916666368061,17.9289321881345,19.4747649179816));
#18314=CARTESIAN_POINT('',(348.987734179926,25.,19.4747649179816));
#18315=CARTESIAN_POINT('',(348.987734179926,25.,19.4747649179816));
#18316=CARTESIAN_POINT('',(356.058801991792,32.0710678118655,19.4747649179816));
#18317=CARTESIAN_POINT('',(348.987734179926,25.,19.4747649179816));
#18318=CARTESIAN_POINT('',(356.058801991792,50.,19.4747649179816));
#18319=CARTESIAN_POINT('',(371.631415464215,25.,19.4747649179816));
#18320=CARTESIAN_POINT('Origin',(373.131415464215,25.,19.4747649179816));
#18321=CARTESIAN_POINT('',(367.006415464215,29.,19.4747649179816));
#18322=CARTESIAN_POINT('Origin',(368.506415464215,29.,19.4747649179816));
#18323=CARTESIAN_POINT('',(357.756415464215,29.,19.4747649179816));
#18324=CARTESIAN_POINT('Origin',(359.256415464215,29.,19.4747649179816));
#18325=CARTESIAN_POINT('',(357.756415464215,25.,19.4747649179816));
#18326=CARTESIAN_POINT('Origin',(359.256415464215,25.,19.4747649179816));
#18327=CARTESIAN_POINT('',(367.006415464215,25.,19.4747649179816));
#18328=CARTESIAN_POINT('Origin',(368.506415464215,25.,19.4747649179816));
#18329=CARTESIAN_POINT('',(362.381415464215,21.,19.4747649179816));
#18330=CARTESIAN_POINT('Origin',(363.881415464215,21.,19.4747649179816));
#18331=CARTESIAN_POINT('',(362.381415464215,25.,19.4747649179816));
#18332=CARTESIAN_POINT('Origin',(363.881415464215,25.,19.4747649179816));
#18333=CARTESIAN_POINT('',(357.756415464215,21.,19.4747649179816));
#18334=CARTESIAN_POINT('Origin',(359.256415464215,21.,19.4747649179816));
#18335=CARTESIAN_POINT('',(367.006415464215,21.,19.4747649179816));
#18336=CARTESIAN_POINT('Origin',(368.506415464215,21.,19.4747649179816));
#18337=CARTESIAN_POINT('',(353.131415464215,25.,19.4747649179816));
#18338=CARTESIAN_POINT('Origin',(354.631415464215,25.,19.4747649179816));
#18339=CARTESIAN_POINT('',(362.381415464215,29.,19.4747649179816));
#18340=CARTESIAN_POINT('Origin',(363.881415464215,29.,19.4747649179816));
#18341=CARTESIAN_POINT('Origin',(373.131415464215,25.,19.4747649179816));
#18342=CARTESIAN_POINT('',(371.631415464215,25.,22.9997649179816));
#18343=CARTESIAN_POINT('Origin',(373.131415464215,25.,22.9997649179816));
#18344=CARTESIAN_POINT('',(371.631415464215,25.,19.4747649179816));
#18345=CARTESIAN_POINT('Origin',(368.506415464215,29.,19.4747649179816));
#18346=CARTESIAN_POINT('',(367.006415464215,29.,22.9997649179816));
#18347=CARTESIAN_POINT('Origin',(368.506415464215,29.,22.9997649179816));
#18348=CARTESIAN_POINT('',(367.006415464215,29.,19.4747649179816));
#18349=CARTESIAN_POINT('Origin',(359.256415464215,29.,19.4747649179816));
#18350=CARTESIAN_POINT('',(357.756415464215,29.,22.9997649179816));
#18351=CARTESIAN_POINT('Origin',(359.256415464215,29.,22.9997649179816));
#18352=CARTESIAN_POINT('',(357.756415464215,29.,19.4747649179816));
#18353=CARTESIAN_POINT('Origin',(359.256415464215,25.,19.4747649179816));
#18354=CARTESIAN_POINT('',(357.756415464215,25.,22.9997649179816));
#18355=CARTESIAN_POINT('Origin',(359.256415464215,25.,22.9997649179816));
#18356=CARTESIAN_POINT('',(357.756415464215,25.,19.4747649179816));
#18357=CARTESIAN_POINT('Origin',(368.506415464215,25.,19.4747649179816));
#18358=CARTESIAN_POINT('',(367.006415464215,25.,22.9997649179816));
#18359=CARTESIAN_POINT('Origin',(368.506415464215,25.,22.9997649179816));
#18360=CARTESIAN_POINT('',(367.006415464215,25.,19.4747649179816));
#18361=CARTESIAN_POINT('Origin',(363.881415464215,21.,19.4747649179816));
#18362=CARTESIAN_POINT('',(362.381415464215,21.,22.9997649179816));
#18363=CARTESIAN_POINT('Origin',(363.881415464215,21.,22.9997649179816));
#18364=CARTESIAN_POINT('',(362.381415464215,21.,19.4747649179816));
#18365=CARTESIAN_POINT('Origin',(363.881415464215,25.,19.4747649179816));
#18366=CARTESIAN_POINT('',(362.381415464215,25.,22.9997649179816));
#18367=CARTESIAN_POINT('Origin',(363.881415464215,25.,22.9997649179816));
#18368=CARTESIAN_POINT('',(362.381415464215,25.,19.4747649179816));
#18369=CARTESIAN_POINT('Origin',(359.256415464215,21.,19.4747649179816));
#18370=CARTESIAN_POINT('',(357.756415464215,21.,22.9997649179816));
#18371=CARTESIAN_POINT('Origin',(359.256415464215,21.,22.9997649179816));
#18372=CARTESIAN_POINT('',(357.756415464215,21.,19.4747649179816));
#18373=CARTESIAN_POINT('Origin',(368.506415464215,21.,19.4747649179816));
#18374=CARTESIAN_POINT('',(367.006415464215,21.,22.9997649179816));
#18375=CARTESIAN_POINT('Origin',(368.506415464215,21.,22.9997649179816));
#18376=CARTESIAN_POINT('',(367.006415464215,21.,19.4747649179816));
#18377=CARTESIAN_POINT('Origin',(354.631415464215,25.,19.4747649179816));
#18378=CARTESIAN_POINT('',(353.131415464215,25.,22.9997649179816));
#18379=CARTESIAN_POINT('Origin',(354.631415464215,25.,22.9997649179816));
#18380=CARTESIAN_POINT('',(353.131415464215,25.,19.4747649179816));
#18381=CARTESIAN_POINT('Origin',(363.881415464215,29.,19.4747649179816));
#18382=CARTESIAN_POINT('',(362.381415464215,29.,22.9997649179816));
#18383=CARTESIAN_POINT('Origin',(363.881415464215,29.,22.9997649179816));
#18384=CARTESIAN_POINT('',(362.381415464215,29.,19.4747649179816));
#18385=CARTESIAN_POINT('Origin',(356.058801991792,32.0710678118655,19.4747649179816));
#18386=CARTESIAN_POINT('',(348.987734179926,25.,22.9997649179816));
#18387=CARTESIAN_POINT('',(348.987734179926,25.,19.4747649179816));
#18388=CARTESIAN_POINT('',(356.058801991792,32.0710678118655,22.9997649179816));
#18389=CARTESIAN_POINT('',(358.889384609376,34.9016504294496,22.9997649179816));
#18390=CARTESIAN_POINT('',(356.058801991792,32.0710678118655,19.4747649179816));
#18391=CARTESIAN_POINT('Origin',(378.987734179926,25.,19.4747649179816));
#18392=CARTESIAN_POINT('',(371.916666368061,32.0710678118655,22.9997649179816));
#18393=CARTESIAN_POINT('',(371.916666368061,32.0710678118655,19.4747649179816));
#18394=CARTESIAN_POINT('',(378.987734179926,25.,22.9997649179816));
#18395=CARTESIAN_POINT('',(372.62161765641,31.3661165235168,22.9997649179816));
#18396=CARTESIAN_POINT('',(378.987734179926,25.,19.4747649179816));
#18397=CARTESIAN_POINT('Origin',(371.916666368061,17.9289321881345,19.4747649179816));
#18398=CARTESIAN_POINT('',(371.916666368061,17.9289321881345,22.9997649179816));
#18399=CARTESIAN_POINT('',(374.31831679751,20.3305826175841,22.9997649179816));
#18400=CARTESIAN_POINT('',(371.916666368061,17.9289321881345,19.4747649179816));
#18401=CARTESIAN_POINT('Origin',(356.058801991792,17.9289321881345,19.4747649179816));
#18402=CARTESIAN_POINT('',(356.058801991792,17.9289321881345,22.9997649179816));
#18403=CARTESIAN_POINT('',(360.023268085859,17.9289321881345,22.9997649179816));
#18404=CARTESIAN_POINT('',(356.058801991792,17.9289321881345,19.4747649179816));
#18405=CARTESIAN_POINT('Origin',(348.987734179926,25.,19.4747649179816));
#18406=CARTESIAN_POINT('',(350.12161765641,23.8661165235168,22.9997649179816));
#18407=CARTESIAN_POINT('Origin',(363.987734179926,35.4644660940673,22.9997649179816));
#18408=CARTESIAN_POINT('',(356.058801991792,50.,22.9997649179816));
#18409=CARTESIAN_POINT('',(371.916666368061,50.,22.9997649179816));
#18410=CARTESIAN_POINT('',(367.952200273994,50.,22.9997649179816));
#18411=CARTESIAN_POINT('',(356.058801991792,44.2322330470336,22.9997649179816));
#18412=CARTESIAN_POINT('',(371.916666368061,33.7677669529664,22.9997649179816));
#18413=CARTESIAN_POINT('Origin',(356.058801991792,53.,30.4747649179816));
#18414=CARTESIAN_POINT('',(356.058801991792,53.,-0.000235082018433808));
#18415=CARTESIAN_POINT('',(356.058801991792,53.,30.4747649179816));
#18416=CARTESIAN_POINT('',(371.916666368061,53.,-0.000235082018433808));
#18417=CARTESIAN_POINT('',(371.916666368061,53.,30.4747649179816));
#18418=CARTESIAN_POINT('',(356.058801991792,53.,-0.000235082018433808));
#18419=CARTESIAN_POINT('Origin',(371.916666368061,50.,30.4747649179816));
#18420=CARTESIAN_POINT('',(356.058801991792,50.,30.4747649179816));
#18421=CARTESIAN_POINT('',(371.916666368061,50.,30.4747649179816));
#18422=CARTESIAN_POINT('Origin',(356.058801991792,50.,30.4747649179816));
#18423=CARTESIAN_POINT('',(356.058801991792,50.,-0.000235082018433808));
#18424=CARTESIAN_POINT('',(356.058801991792,50.,-0.000235082018433808));
#18425=CARTESIAN_POINT('',(356.058801991792,50.,30.4747649179816));
#18426=CARTESIAN_POINT('Origin',(371.916666368061,50.,30.4747649179816));
#18427=CARTESIAN_POINT('',(371.916666368061,50.,-0.000235082018433808));
#18428=CARTESIAN_POINT('',(371.916666368061,50.,-0.000235082018433808));
#18429=CARTESIAN_POINT('',(371.916666368061,50.,30.4747649179816));
#18430=CARTESIAN_POINT('Origin',(371.916666368061,53.,30.4747649179816));
#18431=CARTESIAN_POINT('',(371.916666368061,53.,-0.000235082018433808));
#18432=CARTESIAN_POINT('Origin',(363.987734179926,51.5,-0.000235082018433808));
#18433=CARTESIAN_POINT('',(0.,0.,0.));
#18434=CARTESIAN_POINT('Origin',(363.987734179926,62.5,25.7372649179816));
#18435=CARTESIAN_POINT('',(365.452734179926,60.5,25.7372649179816));
#18436=CARTESIAN_POINT('Origin',(363.987734179926,60.5,25.7372649179816));
#18437=CARTESIAN_POINT('',(365.452734179926,62.5,25.7372649179816));
#18438=CARTESIAN_POINT('',(365.452734179926,62.5,25.7372649179816));
#18439=CARTESIAN_POINT('Origin',(363.987734179926,62.5,25.7372649179816));
#18440=CARTESIAN_POINT('Origin',(361.100982833978,62.5,25.7372649179816));
#18441=CARTESIAN_POINT('',(362.544358506952,62.5,23.2372649179816));
#18442=CARTESIAN_POINT('',(361.100982833978,62.5,25.7372649179816));
#18443=CARTESIAN_POINT('',(362.544358506952,62.5,23.2372649179816));
#18444=CARTESIAN_POINT('',(362.544358506952,60.5,23.2372649179816));
#18445=CARTESIAN_POINT('',(362.544358506952,62.5,23.2372649179816));
#18446=CARTESIAN_POINT('',(361.100982833978,60.5,25.7372649179816));
#18447=CARTESIAN_POINT('',(362.544358506952,60.5,23.2372649179816));
#18448=CARTESIAN_POINT('',(361.100982833978,62.5,25.7372649179816));
#18449=CARTESIAN_POINT('Origin',(362.544358506952,62.5,28.2372649179815));
#18450=CARTESIAN_POINT('',(362.544358506952,62.5,28.2372649179815));
#18451=CARTESIAN_POINT('',(361.100982833978,62.5,25.7372649179816));
#18452=CARTESIAN_POINT('',(362.544358506952,60.5,28.2372649179815));
#18453=CARTESIAN_POINT('',(361.100982833978,60.5,25.7372649179816));
#18454=CARTESIAN_POINT('',(362.544358506952,62.5,28.2372649179815));
#18455=CARTESIAN_POINT('Origin',(365.4311098529,62.5,28.2372649179815));
#18456=CARTESIAN_POINT('',(365.4311098529,62.5,28.2372649179815));
#18457=CARTESIAN_POINT('',(362.544358506952,62.5,28.2372649179815));
#18458=CARTESIAN_POINT('',(365.4311098529,60.5,28.2372649179815));
#18459=CARTESIAN_POINT('',(362.544358506952,60.5,28.2372649179815));
#18460=CARTESIAN_POINT('',(365.4311098529,62.5,28.2372649179815));
#18461=CARTESIAN_POINT('Origin',(366.874485525875,62.5,25.7372649179816));
#18462=CARTESIAN_POINT('',(366.874485525875,62.5,25.7372649179816));
#18463=CARTESIAN_POINT('',(365.4311098529,62.5,28.2372649179815));
#18464=CARTESIAN_POINT('',(366.874485525875,60.5,25.7372649179816));
#18465=CARTESIAN_POINT('',(365.4311098529,60.5,28.2372649179815));
#18466=CARTESIAN_POINT('',(366.874485525875,62.5,25.7372649179816));
#18467=CARTESIAN_POINT('Origin',(365.4311098529,62.5,23.2372649179816));
#18468=CARTESIAN_POINT('',(365.4311098529,62.5,23.2372649179816));
#18469=CARTESIAN_POINT('',(366.874485525875,62.5,25.7372649179816));
#18470=CARTESIAN_POINT('',(365.4311098529,60.5,23.2372649179816));
#18471=CARTESIAN_POINT('',(366.874485525875,60.5,25.7372649179816));
#18472=CARTESIAN_POINT('',(365.4311098529,62.5,23.2372649179816));
#18473=CARTESIAN_POINT('Origin',(362.544358506952,62.5,23.2372649179816));
#18474=CARTESIAN_POINT('',(365.4311098529,62.5,23.2372649179816));
#18475=CARTESIAN_POINT('',(365.4311098529,60.5,23.2372649179816));
#18476=CARTESIAN_POINT('Origin',(363.987734179926,62.5,25.7372649179816));
#18477=CARTESIAN_POINT('Origin',(363.987734179926,60.5,25.7372649179816));
#18478=CARTESIAN_POINT('',(0.,0.,0.));
#18479=CARTESIAN_POINT('Origin',(67.9877341799264,50.,25.7372649179816));
#18480=CARTESIAN_POINT('',(66.4877341799264,50.,25.7372649179816));
#18481=CARTESIAN_POINT('Origin',(67.9877341799264,50.,25.7372649179816));
#18482=CARTESIAN_POINT('',(66.4877341799264,53.,25.7372649179816));
#18483=CARTESIAN_POINT('',(66.4877341799264,50.,25.7372649179816));
#18484=CARTESIAN_POINT('Origin',(67.9877341799264,53.,25.7372649179816));
#18485=CARTESIAN_POINT('Origin',(72.0217856971541,53.,3.89451831659521));
#18486=CARTESIAN_POINT('',(74.0217856971541,53.,3.89451831659521));
#18487=CARTESIAN_POINT('Origin',(72.0217856971541,53.,3.89451831659521));
#18488=CARTESIAN_POINT('',(74.0217856971541,50.,3.89451831659521));
#18489=CARTESIAN_POINT('',(74.0217856971541,53.,3.89451831659521));
#18490=CARTESIAN_POINT('Origin',(72.0217856971541,50.,3.89451831659521));
#18491=CARTESIAN_POINT('Origin',(64.0217856971541,53.,3.89451831659521));
#18492=CARTESIAN_POINT('',(66.0217856971541,53.,3.89451831659521));
#18493=CARTESIAN_POINT('Origin',(64.0217856971541,53.,3.89451831659521));
#18494=CARTESIAN_POINT('',(66.0217856971541,50.,3.89451831659521));
#18495=CARTESIAN_POINT('',(66.0217856971541,53.,3.89451831659521));
#18496=CARTESIAN_POINT('Origin',(64.0217856971541,50.,3.89451831659521));
#18497=CARTESIAN_POINT('Origin',(71.9522002739937,48.,28.4747649179816));
#18498=CARTESIAN_POINT('',(75.916666368061,50.,28.4747649179816));
#18499=CARTESIAN_POINT('',(75.916666368061,48.,30.4747649179816));
#18500=CARTESIAN_POINT('Origin',(75.916666368061,48.,28.4747649179816));
#18501=CARTESIAN_POINT('',(60.0588019917919,48.,30.4747649179816));
#18502=CARTESIAN_POINT('',(71.9522002739937,48.,30.4747649179816));
#18503=CARTESIAN_POINT('',(60.0588019917919,50.,28.4747649179816));
#18504=CARTESIAN_POINT('Origin',(60.0588019917919,48.,28.4747649179816));
#18505=CARTESIAN_POINT('',(71.9522002739937,50.,28.4747649179816));
#18506=CARTESIAN_POINT('Origin',(67.9877341799264,35.4644660940673,30.4747649179816));
#18507=CARTESIAN_POINT('',(75.916666368061,32.0710678118655,30.4747649179816));
#18508=CARTESIAN_POINT('',(75.916666368061,50.,30.4747649179816));
#18509=CARTESIAN_POINT('',(82.9877341799264,25.,30.4747649179816));
#18510=CARTESIAN_POINT('',(82.9877341799264,25.,30.4747649179816));
#18511=CARTESIAN_POINT('',(75.916666368061,17.9289321881345,30.4747649179816));
#18512=CARTESIAN_POINT('',(82.9877341799264,25.,30.4747649179816));
#18513=CARTESIAN_POINT('',(60.0588019917919,17.9289321881345,30.4747649179816));
#18514=CARTESIAN_POINT('',(75.916666368061,17.9289321881345,30.4747649179816));
#18515=CARTESIAN_POINT('',(52.9877341799264,25.,30.4747649179816));
#18516=CARTESIAN_POINT('',(52.9877341799264,25.,30.4747649179816));
#18517=CARTESIAN_POINT('',(60.0588019917919,32.0710678118655,30.4747649179816));
#18518=CARTESIAN_POINT('',(52.9877341799264,25.,30.4747649179816));
#18519=CARTESIAN_POINT('',(60.0588019917919,50.,30.4747649179816));
#18520=CARTESIAN_POINT('',(66.3814154642151,29.,30.4747649179816));
#18521=CARTESIAN_POINT('Origin',(67.8814154642151,29.,30.4747649179816));
#18522=CARTESIAN_POINT('',(57.131415464215,25.,30.4747649179816));
#18523=CARTESIAN_POINT('Origin',(58.631415464215,25.,30.4747649179816));
#18524=CARTESIAN_POINT('',(71.0064154642151,21.,30.4747649179816));
#18525=CARTESIAN_POINT('Origin',(72.5064154642151,21.,30.4747649179816));
#18526=CARTESIAN_POINT('',(61.756415464215,21.,30.4747649179816));
#18527=CARTESIAN_POINT('Origin',(63.256415464215,21.,30.4747649179816));
#18528=CARTESIAN_POINT('',(66.3814154642151,25.,30.4747649179816));
#18529=CARTESIAN_POINT('Origin',(67.8814154642151,25.,30.4747649179816));
#18530=CARTESIAN_POINT('',(66.3814154642151,21.,30.4747649179816));
#18531=CARTESIAN_POINT('Origin',(67.8814154642151,21.,30.4747649179816));
#18532=CARTESIAN_POINT('',(71.0064154642151,25.,30.4747649179816));
#18533=CARTESIAN_POINT('Origin',(72.5064154642151,25.,30.4747649179816));
#18534=CARTESIAN_POINT('',(61.756415464215,25.,30.4747649179816));
#18535=CARTESIAN_POINT('Origin',(63.256415464215,25.,30.4747649179816));
#18536=CARTESIAN_POINT('',(61.756415464215,29.,30.4747649179816));
#18537=CARTESIAN_POINT('Origin',(63.256415464215,29.,30.4747649179816));
#18538=CARTESIAN_POINT('',(71.0064154642151,29.,30.4747649179816));
#18539=CARTESIAN_POINT('Origin',(72.5064154642151,29.,30.4747649179816));
#18540=CARTESIAN_POINT('',(75.6314154642151,25.,30.4747649179816));
#18541=CARTESIAN_POINT('Origin',(77.131415464215,25.,30.4747649179816));
#18542=CARTESIAN_POINT('Origin',(60.0588019917919,49.0313730334031,29.9747649179816));
#18543=CARTESIAN_POINT('',(60.0588019917919,53.,30.4747649179816));
#18544=CARTESIAN_POINT('',(60.0588019917919,49.0313730334031,33.9747649179816));
#18545=CARTESIAN_POINT('Origin',(60.0588019917919,49.0313730334031,29.9747649179816));
#18546=CARTESIAN_POINT('',(75.916666368061,49.0313730334031,33.9747649179816));
#18547=CARTESIAN_POINT('',(60.0588019917919,49.0313730334031,33.9747649179816));
#18548=CARTESIAN_POINT('',(75.916666368061,53.,30.4747649179816));
#18549=CARTESIAN_POINT('Origin',(75.916666368061,49.0313730334031,29.9747649179816));
#18550=CARTESIAN_POINT('',(60.0588019917919,53.,30.4747649179816));
#18551=CARTESIAN_POINT('Origin',(67.9877341799264,35.4644660940673,33.9747649179816));
#18552=CARTESIAN_POINT('',(60.0588019917919,32.0710678118655,33.9747649179816));
#18553=CARTESIAN_POINT('',(60.0588019917919,50.,33.9747649179816));
#18554=CARTESIAN_POINT('',(52.9877341799264,25.,33.9747649179816));
#18555=CARTESIAN_POINT('',(52.9877341799264,25.,33.9747649179816));
#18556=CARTESIAN_POINT('',(60.0588019917919,17.9289321881345,33.9747649179816));
#18557=CARTESIAN_POINT('',(52.9877341799264,25.,33.9747649179816));
#18558=CARTESIAN_POINT('',(75.916666368061,17.9289321881345,33.9747649179816));
#18559=CARTESIAN_POINT('',(75.916666368061,17.9289321881345,33.9747649179816));
#18560=CARTESIAN_POINT('',(82.9877341799264,25.,33.9747649179816));
#18561=CARTESIAN_POINT('',(82.9877341799264,25.,33.9747649179816));
#18562=CARTESIAN_POINT('',(75.916666368061,32.0710678118655,33.9747649179816));
#18563=CARTESIAN_POINT('',(82.9877341799264,25.,33.9747649179816));
#18564=CARTESIAN_POINT('',(75.916666368061,50.,33.9747649179816));
#18565=CARTESIAN_POINT('',(75.6314154642151,25.,33.9747649179816));
#18566=CARTESIAN_POINT('Origin',(77.131415464215,25.,33.9747649179816));
#18567=CARTESIAN_POINT('',(71.0064154642151,29.,33.9747649179816));
#18568=CARTESIAN_POINT('Origin',(72.5064154642151,29.,33.9747649179816));
#18569=CARTESIAN_POINT('',(61.756415464215,29.,33.9747649179816));
#18570=CARTESIAN_POINT('Origin',(63.256415464215,29.,33.9747649179816));
#18571=CARTESIAN_POINT('',(61.756415464215,25.,33.9747649179816));
#18572=CARTESIAN_POINT('Origin',(63.256415464215,25.,33.9747649179816));
#18573=CARTESIAN_POINT('',(71.0064154642151,25.,33.9747649179816));
#18574=CARTESIAN_POINT('Origin',(72.5064154642151,25.,33.9747649179816));
#18575=CARTESIAN_POINT('',(66.3814154642151,21.,33.9747649179816));
#18576=CARTESIAN_POINT('Origin',(67.8814154642151,21.,33.9747649179816));
#18577=CARTESIAN_POINT('',(66.3814154642151,25.,33.9747649179816));
#18578=CARTESIAN_POINT('Origin',(67.8814154642151,25.,33.9747649179816));
#18579=CARTESIAN_POINT('',(61.756415464215,21.,33.9747649179816));
#18580=CARTESIAN_POINT('Origin',(63.256415464215,21.,33.9747649179816));
#18581=CARTESIAN_POINT('',(71.0064154642151,21.,33.9747649179816));
#18582=CARTESIAN_POINT('Origin',(72.5064154642151,21.,33.9747649179816));
#18583=CARTESIAN_POINT('',(57.131415464215,25.,33.9747649179816));
#18584=CARTESIAN_POINT('Origin',(58.631415464215,25.,33.9747649179816));
#18585=CARTESIAN_POINT('',(66.3814154642151,29.,33.9747649179816));
#18586=CARTESIAN_POINT('Origin',(67.8814154642151,29.,33.9747649179816));
#18587=CARTESIAN_POINT('Origin',(77.131415464215,25.,30.4747649179816));
#18588=CARTESIAN_POINT('',(75.6314154642151,25.,30.4747649179816));
#18589=CARTESIAN_POINT('Origin',(72.5064154642151,29.,30.4747649179816));
#18590=CARTESIAN_POINT('',(71.0064154642151,29.,30.4747649179816));
#18591=CARTESIAN_POINT('Origin',(63.256415464215,29.,30.4747649179816));
#18592=CARTESIAN_POINT('',(61.756415464215,29.,30.4747649179816));
#18593=CARTESIAN_POINT('Origin',(63.256415464215,25.,30.4747649179816));
#18594=CARTESIAN_POINT('',(61.756415464215,25.,30.4747649179816));
#18595=CARTESIAN_POINT('Origin',(72.5064154642151,25.,30.4747649179816));
#18596=CARTESIAN_POINT('',(71.0064154642151,25.,30.4747649179816));
#18597=CARTESIAN_POINT('Origin',(67.8814154642151,21.,30.4747649179816));
#18598=CARTESIAN_POINT('',(66.3814154642151,21.,30.4747649179816));
#18599=CARTESIAN_POINT('Origin',(67.8814154642151,25.,30.4747649179816));
#18600=CARTESIAN_POINT('',(66.3814154642151,25.,30.4747649179816));
#18601=CARTESIAN_POINT('Origin',(63.256415464215,21.,30.4747649179816));
#18602=CARTESIAN_POINT('',(61.756415464215,21.,30.4747649179816));
#18603=CARTESIAN_POINT('Origin',(72.5064154642151,21.,30.4747649179816));
#18604=CARTESIAN_POINT('',(71.0064154642151,21.,30.4747649179816));
#18605=CARTESIAN_POINT('Origin',(58.631415464215,25.,30.4747649179816));
#18606=CARTESIAN_POINT('',(57.131415464215,25.,30.4747649179816));
#18607=CARTESIAN_POINT('Origin',(67.8814154642151,29.,30.4747649179816));
#18608=CARTESIAN_POINT('',(66.3814154642151,29.,30.4747649179816));
#18609=CARTESIAN_POINT('Origin',(60.0588019917919,32.0710678118655,30.4747649179816));
#18610=CARTESIAN_POINT('',(52.9877341799264,25.,30.4747649179816));
#18611=CARTESIAN_POINT('',(60.0588019917919,32.0710678118655,30.4747649179816));
#18612=CARTESIAN_POINT('Origin',(82.9877341799264,25.,30.4747649179816));
#18613=CARTESIAN_POINT('',(75.916666368061,32.0710678118655,30.4747649179816));
#18614=CARTESIAN_POINT('',(82.9877341799264,25.,30.4747649179816));
#18615=CARTESIAN_POINT('Origin',(75.916666368061,17.9289321881345,30.4747649179816));
#18616=CARTESIAN_POINT('',(75.916666368061,17.9289321881345,30.4747649179816));
#18617=CARTESIAN_POINT('Origin',(60.0588019917919,17.9289321881345,30.4747649179816));
#18618=CARTESIAN_POINT('',(60.0588019917919,17.9289321881345,30.4747649179816));
#18619=CARTESIAN_POINT('Origin',(52.9877341799264,25.,30.4747649179816));
#18620=CARTESIAN_POINT('Origin',(67.9877341799264,35.4644660940673,19.4747649179816));
#18621=CARTESIAN_POINT('',(75.916666368061,50.,19.4747649179816));
#18622=CARTESIAN_POINT('',(60.0588019917919,50.,19.4747649179816));
#18623=CARTESIAN_POINT('',(71.9522002739937,50.,19.4747649179816));
#18624=CARTESIAN_POINT('',(75.916666368061,32.0710678118655,19.4747649179816));
#18625=CARTESIAN_POINT('',(75.916666368061,50.,19.4747649179816));
#18626=CARTESIAN_POINT('',(82.9877341799264,25.,19.4747649179816));
#18627=CARTESIAN_POINT('',(82.9877341799264,25.,19.4747649179816));
#18628=CARTESIAN_POINT('',(75.916666368061,17.9289321881345,19.4747649179816));
#18629=CARTESIAN_POINT('',(82.9877341799264,25.,19.4747649179816));
#18630=CARTESIAN_POINT('',(60.0588019917919,17.9289321881345,19.4747649179816));
#18631=CARTESIAN_POINT('',(75.916666368061,17.9289321881345,19.4747649179816));
#18632=CARTESIAN_POINT('',(52.9877341799264,25.,19.4747649179816));
#18633=CARTESIAN_POINT('',(52.9877341799264,25.,19.4747649179816));
#18634=CARTESIAN_POINT('',(60.0588019917919,32.0710678118655,19.4747649179816));
#18635=CARTESIAN_POINT('',(52.9877341799264,25.,19.4747649179816));
#18636=CARTESIAN_POINT('',(60.0588019917919,50.,19.4747649179816));
#18637=CARTESIAN_POINT('',(75.6314154642151,25.,19.4747649179816));
#18638=CARTESIAN_POINT('Origin',(77.131415464215,25.,19.4747649179816));
#18639=CARTESIAN_POINT('',(71.0064154642151,29.,19.4747649179816));
#18640=CARTESIAN_POINT('Origin',(72.5064154642151,29.,19.4747649179816));
#18641=CARTESIAN_POINT('',(61.756415464215,29.,19.4747649179816));
#18642=CARTESIAN_POINT('Origin',(63.256415464215,29.,19.4747649179816));
#18643=CARTESIAN_POINT('',(61.756415464215,25.,19.4747649179816));
#18644=CARTESIAN_POINT('Origin',(63.256415464215,25.,19.4747649179816));
#18645=CARTESIAN_POINT('',(71.0064154642151,25.,19.4747649179816));
#18646=CARTESIAN_POINT('Origin',(72.5064154642151,25.,19.4747649179816));
#18647=CARTESIAN_POINT('',(66.3814154642151,21.,19.4747649179816));
#18648=CARTESIAN_POINT('Origin',(67.8814154642151,21.,19.4747649179816));
#18649=CARTESIAN_POINT('',(66.3814154642151,25.,19.4747649179816));
#18650=CARTESIAN_POINT('Origin',(67.8814154642151,25.,19.4747649179816));
#18651=CARTESIAN_POINT('',(61.756415464215,21.,19.4747649179816));
#18652=CARTESIAN_POINT('Origin',(63.256415464215,21.,19.4747649179816));
#18653=CARTESIAN_POINT('',(71.0064154642151,21.,19.4747649179816));
#18654=CARTESIAN_POINT('Origin',(72.5064154642151,21.,19.4747649179816));
#18655=CARTESIAN_POINT('',(57.131415464215,25.,19.4747649179816));
#18656=CARTESIAN_POINT('Origin',(58.631415464215,25.,19.4747649179816));
#18657=CARTESIAN_POINT('',(66.3814154642151,29.,19.4747649179816));
#18658=CARTESIAN_POINT('Origin',(67.8814154642151,29.,19.4747649179816));
#18659=CARTESIAN_POINT('Origin',(77.131415464215,25.,19.4747649179816));
#18660=CARTESIAN_POINT('',(75.6314154642151,25.,22.9997649179816));
#18661=CARTESIAN_POINT('Origin',(77.131415464215,25.,22.9997649179816));
#18662=CARTESIAN_POINT('',(75.6314154642151,25.,19.4747649179816));
#18663=CARTESIAN_POINT('Origin',(72.5064154642151,29.,19.4747649179816));
#18664=CARTESIAN_POINT('',(71.0064154642151,29.,22.9997649179816));
#18665=CARTESIAN_POINT('Origin',(72.5064154642151,29.,22.9997649179816));
#18666=CARTESIAN_POINT('',(71.0064154642151,29.,19.4747649179816));
#18667=CARTESIAN_POINT('Origin',(63.256415464215,29.,19.4747649179816));
#18668=CARTESIAN_POINT('',(61.756415464215,29.,22.9997649179816));
#18669=CARTESIAN_POINT('Origin',(63.256415464215,29.,22.9997649179816));
#18670=CARTESIAN_POINT('',(61.756415464215,29.,19.4747649179816));
#18671=CARTESIAN_POINT('Origin',(63.256415464215,25.,19.4747649179816));
#18672=CARTESIAN_POINT('',(61.756415464215,25.,22.9997649179816));
#18673=CARTESIAN_POINT('Origin',(63.256415464215,25.,22.9997649179816));
#18674=CARTESIAN_POINT('',(61.756415464215,25.,19.4747649179816));
#18675=CARTESIAN_POINT('Origin',(72.5064154642151,25.,19.4747649179816));
#18676=CARTESIAN_POINT('',(71.0064154642151,25.,22.9997649179816));
#18677=CARTESIAN_POINT('Origin',(72.5064154642151,25.,22.9997649179816));
#18678=CARTESIAN_POINT('',(71.0064154642151,25.,19.4747649179816));
#18679=CARTESIAN_POINT('Origin',(67.8814154642151,21.,19.4747649179816));
#18680=CARTESIAN_POINT('',(66.3814154642151,21.,22.9997649179816));
#18681=CARTESIAN_POINT('Origin',(67.8814154642151,21.,22.9997649179816));
#18682=CARTESIAN_POINT('',(66.3814154642151,21.,19.4747649179816));
#18683=CARTESIAN_POINT('Origin',(67.8814154642151,25.,19.4747649179816));
#18684=CARTESIAN_POINT('',(66.3814154642151,25.,22.9997649179816));
#18685=CARTESIAN_POINT('Origin',(67.8814154642151,25.,22.9997649179816));
#18686=CARTESIAN_POINT('',(66.3814154642151,25.,19.4747649179816));
#18687=CARTESIAN_POINT('Origin',(63.256415464215,21.,19.4747649179816));
#18688=CARTESIAN_POINT('',(61.756415464215,21.,22.9997649179816));
#18689=CARTESIAN_POINT('Origin',(63.256415464215,21.,22.9997649179816));
#18690=CARTESIAN_POINT('',(61.756415464215,21.,19.4747649179816));
#18691=CARTESIAN_POINT('Origin',(72.5064154642151,21.,19.4747649179816));
#18692=CARTESIAN_POINT('',(71.0064154642151,21.,22.9997649179816));
#18693=CARTESIAN_POINT('Origin',(72.5064154642151,21.,22.9997649179816));
#18694=CARTESIAN_POINT('',(71.0064154642151,21.,19.4747649179816));
#18695=CARTESIAN_POINT('Origin',(58.631415464215,25.,19.4747649179816));
#18696=CARTESIAN_POINT('',(57.131415464215,25.,22.9997649179816));
#18697=CARTESIAN_POINT('Origin',(58.631415464215,25.,22.9997649179816));
#18698=CARTESIAN_POINT('',(57.131415464215,25.,19.4747649179816));
#18699=CARTESIAN_POINT('Origin',(67.8814154642151,29.,19.4747649179816));
#18700=CARTESIAN_POINT('',(66.3814154642151,29.,22.9997649179816));
#18701=CARTESIAN_POINT('Origin',(67.8814154642151,29.,22.9997649179816));
#18702=CARTESIAN_POINT('',(66.3814154642151,29.,19.4747649179816));
#18703=CARTESIAN_POINT('Origin',(60.0588019917919,32.0710678118655,19.4747649179816));
#18704=CARTESIAN_POINT('',(52.9877341799264,25.,22.9997649179816));
#18705=CARTESIAN_POINT('',(52.9877341799264,25.,19.4747649179816));
#18706=CARTESIAN_POINT('',(60.0588019917919,32.0710678118655,22.9997649179816));
#18707=CARTESIAN_POINT('',(62.8893846093759,34.9016504294496,22.9997649179816));
#18708=CARTESIAN_POINT('',(60.0588019917919,32.0710678118655,19.4747649179816));
#18709=CARTESIAN_POINT('Origin',(82.9877341799264,25.,19.4747649179816));
#18710=CARTESIAN_POINT('',(75.916666368061,32.0710678118655,22.9997649179816));
#18711=CARTESIAN_POINT('',(75.916666368061,32.0710678118655,19.4747649179816));
#18712=CARTESIAN_POINT('',(82.9877341799264,25.,22.9997649179816));
#18713=CARTESIAN_POINT('',(76.6216176564096,31.3661165235168,22.9997649179816));
#18714=CARTESIAN_POINT('',(82.9877341799264,25.,19.4747649179816));
#18715=CARTESIAN_POINT('Origin',(75.916666368061,17.9289321881345,19.4747649179816));
#18716=CARTESIAN_POINT('',(75.916666368061,17.9289321881345,22.9997649179816));
#18717=CARTESIAN_POINT('',(78.3183167975105,20.3305826175841,22.9997649179816));
#18718=CARTESIAN_POINT('',(75.916666368061,17.9289321881345,19.4747649179816));
#18719=CARTESIAN_POINT('Origin',(60.0588019917919,17.9289321881345,19.4747649179816));
#18720=CARTESIAN_POINT('',(60.0588019917919,17.9289321881345,22.9997649179816));
#18721=CARTESIAN_POINT('',(64.0232680858592,17.9289321881345,22.9997649179816));
#18722=CARTESIAN_POINT('',(60.0588019917919,17.9289321881345,19.4747649179816));
#18723=CARTESIAN_POINT('Origin',(52.9877341799264,25.,19.4747649179816));
#18724=CARTESIAN_POINT('',(54.1216176564096,23.8661165235168,22.9997649179816));
#18725=CARTESIAN_POINT('Origin',(67.9877341799264,35.4644660940673,22.9997649179816));
#18726=CARTESIAN_POINT('',(60.0588019917919,50.,22.9997649179816));
#18727=CARTESIAN_POINT('',(75.916666368061,50.,22.9997649179816));
#18728=CARTESIAN_POINT('',(71.9522002739937,50.,22.9997649179816));
#18729=CARTESIAN_POINT('',(60.0588019917919,44.2322330470336,22.9997649179816));
#18730=CARTESIAN_POINT('',(75.916666368061,33.7677669529664,22.9997649179816));
#18731=CARTESIAN_POINT('Origin',(60.0588019917919,53.,30.4747649179816));
#18732=CARTESIAN_POINT('',(60.0588019917919,53.,-0.000235082018433808));
#18733=CARTESIAN_POINT('',(60.0588019917919,53.,30.4747649179816));
#18734=CARTESIAN_POINT('',(75.916666368061,53.,-0.000235082018433808));
#18735=CARTESIAN_POINT('',(75.916666368061,53.,30.4747649179816));
#18736=CARTESIAN_POINT('',(60.0588019917919,53.,-0.000235082018433808));
#18737=CARTESIAN_POINT('Origin',(75.916666368061,50.,30.4747649179816));
#18738=CARTESIAN_POINT('',(60.0588019917919,50.,30.4747649179816));
#18739=CARTESIAN_POINT('',(75.916666368061,50.,30.4747649179816));
#18740=CARTESIAN_POINT('Origin',(60.0588019917919,50.,30.4747649179816));
#18741=CARTESIAN_POINT('',(60.0588019917919,50.,-0.000235082018433808));
#18742=CARTESIAN_POINT('',(60.0588019917919,50.,-0.000235082018433808));
#18743=CARTESIAN_POINT('',(60.0588019917919,50.,30.4747649179816));
#18744=CARTESIAN_POINT('Origin',(75.916666368061,50.,30.4747649179816));
#18745=CARTESIAN_POINT('',(75.916666368061,50.,-0.000235082018433808));
#18746=CARTESIAN_POINT('',(75.916666368061,50.,-0.000235082018433808));
#18747=CARTESIAN_POINT('',(75.916666368061,50.,30.4747649179816));
#18748=CARTESIAN_POINT('Origin',(75.916666368061,53.,30.4747649179816));
#18749=CARTESIAN_POINT('',(75.916666368061,53.,-0.000235082018433808));
#18750=CARTESIAN_POINT('Origin',(67.9877341799264,51.5,-0.000235082018433808));
#18751=CARTESIAN_POINT('',(0.,0.,0.));
#18752=CARTESIAN_POINT('Origin',(67.9877341799264,50.,25.7372649179816));
#18753=CARTESIAN_POINT('',(69.3018338062367,50.,23.8381926430366));
#18754=CARTESIAN_POINT('',(70.2894288268066,50.,25.9257724399974));
#18755=CARTESIAN_POINT('',(69.3018338062367,50.,23.8381926430366));
#18756=CARTESIAN_POINT('',(67.0001391593565,50.,23.6496851210208));
#18757=CARTESIAN_POINT('',(67.0001391593565,50.,23.6496851210208));
#18758=CARTESIAN_POINT('',(65.6860395330462,50.,25.5487573959657));
#18759=CARTESIAN_POINT('',(65.6860395330462,50.,25.5487573959657));
#18760=CARTESIAN_POINT('',(66.6736345536162,50.,27.6363371929265));
#18761=CARTESIAN_POINT('',(66.6736345536162,50.,27.6363371929265));
#18762=CARTESIAN_POINT('',(68.9753292004963,50.,27.8248447149424));
#18763=CARTESIAN_POINT('',(68.9753292004963,50.,27.8248447149424));
#18764=CARTESIAN_POINT('',(70.2894288268066,50.,25.9257724399974));
#18765=CARTESIAN_POINT('',(66.5242341799264,50.,25.7372649179816));
#18766=CARTESIAN_POINT('Origin',(67.9877341799264,50.,25.7372649179816));
#18767=CARTESIAN_POINT('Origin',(67.0001391593565,50.,23.6496851210208));
#18768=CARTESIAN_POINT('',(69.3018338062367,49.,23.8381926430366));
#18769=CARTESIAN_POINT('',(69.3018338062367,50.,23.8381926430366));
#18770=CARTESIAN_POINT('',(67.0001391593565,49.,23.6496851210208));
#18771=CARTESIAN_POINT('',(67.0001391593565,49.,23.6496851210208));
#18772=CARTESIAN_POINT('',(67.0001391593565,50.,23.6496851210208));
#18773=CARTESIAN_POINT('Origin',(65.6860395330462,50.,25.5487573959657));
#18774=CARTESIAN_POINT('',(65.6860395330462,49.,25.5487573959657));
#18775=CARTESIAN_POINT('',(65.6860395330462,49.,25.5487573959657));
#18776=CARTESIAN_POINT('',(65.6860395330462,50.,25.5487573959657));
#18777=CARTESIAN_POINT('Origin',(66.6736345536162,50.,27.6363371929265));
#18778=CARTESIAN_POINT('',(66.6736345536162,49.,27.6363371929265));
#18779=CARTESIAN_POINT('',(66.6736345536162,49.,27.6363371929265));
#18780=CARTESIAN_POINT('',(66.6736345536162,50.,27.6363371929265));
#18781=CARTESIAN_POINT('Origin',(68.9753292004963,50.,27.8248447149424));
#18782=CARTESIAN_POINT('',(68.9753292004963,49.,27.8248447149424));
#18783=CARTESIAN_POINT('',(68.9753292004963,49.,27.8248447149424));
#18784=CARTESIAN_POINT('',(68.9753292004963,50.,27.8248447149424));
#18785=CARTESIAN_POINT('Origin',(70.2894288268066,50.,25.9257724399974));
#18786=CARTESIAN_POINT('',(70.2894288268066,49.,25.9257724399974));
#18787=CARTESIAN_POINT('',(70.2894288268066,49.,25.9257724399974));
#18788=CARTESIAN_POINT('',(70.2894288268066,50.,25.9257724399974));
#18789=CARTESIAN_POINT('Origin',(69.3018338062367,50.,23.8381926430366));
#18790=CARTESIAN_POINT('',(69.3018338062367,49.,23.8381926430366));
#18791=CARTESIAN_POINT('Origin',(67.9877341799264,49.,25.7372649179816));
#18792=CARTESIAN_POINT('Origin',(67.9877341799264,50.,25.7372649179816));
#18793=CARTESIAN_POINT('',(66.5242341799264,63.,25.7372649179816));
#18794=CARTESIAN_POINT('Origin',(67.9877341799264,63.,25.7372649179816));
#18795=CARTESIAN_POINT('',(66.5242341799264,50.,25.7372649179816));
#18796=CARTESIAN_POINT('Origin',(67.9877341799264,63.,25.7372649179816));
#18797=CARTESIAN_POINT('',(0.,0.,0.));
#18798=CARTESIAN_POINT('Origin',(363.987734179926,58.5,25.7372649179816));
#18799=CARTESIAN_POINT('',(365.452734179926,56.5,25.7372649179816));
#18800=CARTESIAN_POINT('Origin',(363.987734179926,56.5,25.7372649179816));
#18801=CARTESIAN_POINT('',(365.452734179926,58.5,25.7372649179816));
#18802=CARTESIAN_POINT('',(365.452734179926,58.5,25.7372649179816));
#18803=CARTESIAN_POINT('Origin',(363.987734179926,58.5,25.7372649179816));
#18804=CARTESIAN_POINT('Origin',(361.100982833978,58.5,25.7372649179816));
#18805=CARTESIAN_POINT('',(362.544358506952,58.5,23.2372649179816));
#18806=CARTESIAN_POINT('',(361.100982833978,58.5,25.7372649179816));
#18807=CARTESIAN_POINT('',(362.544358506952,58.5,23.2372649179816));
#18808=CARTESIAN_POINT('',(362.544358506952,56.5,23.2372649179816));
#18809=CARTESIAN_POINT('',(362.544358506952,58.5,23.2372649179816));
#18810=CARTESIAN_POINT('',(361.100982833978,56.5,25.7372649179816));
#18811=CARTESIAN_POINT('',(362.544358506952,56.5,23.2372649179816));
#18812=CARTESIAN_POINT('',(361.100982833978,58.5,25.7372649179816));
#18813=CARTESIAN_POINT('Origin',(362.544358506952,58.5,28.2372649179815));
#18814=CARTESIAN_POINT('',(362.544358506952,58.5,28.2372649179815));
#18815=CARTESIAN_POINT('',(361.100982833978,58.5,25.7372649179816));
#18816=CARTESIAN_POINT('',(362.544358506952,56.5,28.2372649179815));
#18817=CARTESIAN_POINT('',(361.100982833978,56.5,25.7372649179816));
#18818=CARTESIAN_POINT('',(362.544358506952,58.5,28.2372649179815));
#18819=CARTESIAN_POINT('Origin',(365.4311098529,58.5,28.2372649179815));
#18820=CARTESIAN_POINT('',(365.4311098529,58.5,28.2372649179815));
#18821=CARTESIAN_POINT('',(362.544358506952,58.5,28.2372649179815));
#18822=CARTESIAN_POINT('',(365.4311098529,56.5,28.2372649179815));
#18823=CARTESIAN_POINT('',(362.544358506952,56.5,28.2372649179815));
#18824=CARTESIAN_POINT('',(365.4311098529,58.5,28.2372649179815));
#18825=CARTESIAN_POINT('Origin',(366.874485525875,58.5,25.7372649179816));
#18826=CARTESIAN_POINT('',(366.874485525875,58.5,25.7372649179816));
#18827=CARTESIAN_POINT('',(365.4311098529,58.5,28.2372649179815));
#18828=CARTESIAN_POINT('',(366.874485525875,56.5,25.7372649179816));
#18829=CARTESIAN_POINT('',(365.4311098529,56.5,28.2372649179815));
#18830=CARTESIAN_POINT('',(366.874485525875,58.5,25.7372649179816));
#18831=CARTESIAN_POINT('Origin',(365.4311098529,58.5,23.2372649179816));
#18832=CARTESIAN_POINT('',(365.4311098529,58.5,23.2372649179816));
#18833=CARTESIAN_POINT('',(366.874485525875,58.5,25.7372649179816));
#18834=CARTESIAN_POINT('',(365.4311098529,56.5,23.2372649179816));
#18835=CARTESIAN_POINT('',(366.874485525875,56.5,25.7372649179816));
#18836=CARTESIAN_POINT('',(365.4311098529,58.5,23.2372649179816));
#18837=CARTESIAN_POINT('Origin',(362.544358506952,58.5,23.2372649179816));
#18838=CARTESIAN_POINT('',(365.4311098529,58.5,23.2372649179816));
#18839=CARTESIAN_POINT('',(365.4311098529,56.5,23.2372649179816));
#18840=CARTESIAN_POINT('Origin',(363.987734179926,58.5,25.7372649179816));
#18841=CARTESIAN_POINT('Origin',(363.987734179926,56.5,25.7372649179816));
#18842=CARTESIAN_POINT('',(0.,0.,0.));
#18843=CARTESIAN_POINT('Origin',(67.9877341799264,58.5,25.7372649179816));
#18844=CARTESIAN_POINT('',(69.4527341799265,56.5,25.7372649179816));
#18845=CARTESIAN_POINT('Origin',(67.9877341799264,56.5,25.7372649179816));
#18846=CARTESIAN_POINT('',(69.4527341799265,58.5,25.7372649179816));
#18847=CARTESIAN_POINT('',(69.4527341799264,58.5,25.7372649179816));
#18848=CARTESIAN_POINT('Origin',(67.9877341799264,58.5,25.7372649179816));
#18849=CARTESIAN_POINT('Origin',(65.1009828339783,58.5,25.7372649179816));
#18850=CARTESIAN_POINT('',(66.5443585069524,58.5,23.2372649179816));
#18851=CARTESIAN_POINT('',(65.1009828339783,58.5,25.7372649179816));
#18852=CARTESIAN_POINT('',(66.5443585069524,58.5,23.2372649179816));
#18853=CARTESIAN_POINT('',(66.5443585069524,56.5,23.2372649179816));
#18854=CARTESIAN_POINT('',(66.5443585069524,58.5,23.2372649179816));
#18855=CARTESIAN_POINT('',(65.1009828339783,56.5,25.7372649179816));
#18856=CARTESIAN_POINT('',(66.5443585069524,56.5,23.2372649179816));
#18857=CARTESIAN_POINT('',(65.1009828339783,58.5,25.7372649179816));
#18858=CARTESIAN_POINT('Origin',(66.5443585069524,58.5,28.2372649179815));
#18859=CARTESIAN_POINT('',(66.5443585069524,58.5,28.2372649179815));
#18860=CARTESIAN_POINT('',(65.1009828339783,58.5,25.7372649179816));
#18861=CARTESIAN_POINT('',(66.5443585069524,56.5,28.2372649179815));
#18862=CARTESIAN_POINT('',(65.1009828339783,56.5,25.7372649179816));
#18863=CARTESIAN_POINT('',(66.5443585069524,58.5,28.2372649179815));
#18864=CARTESIAN_POINT('Origin',(69.4311098529005,58.5,28.2372649179815));
#18865=CARTESIAN_POINT('',(69.4311098529005,58.5,28.2372649179815));
#18866=CARTESIAN_POINT('',(66.5443585069524,58.5,28.2372649179815));
#18867=CARTESIAN_POINT('',(69.4311098529005,56.5,28.2372649179815));
#18868=CARTESIAN_POINT('',(66.5443585069524,56.5,28.2372649179815));
#18869=CARTESIAN_POINT('',(69.4311098529005,58.5,28.2372649179815));
#18870=CARTESIAN_POINT('Origin',(70.8744855258745,58.5,25.7372649179816));
#18871=CARTESIAN_POINT('',(70.8744855258745,58.5,25.7372649179816));
#18872=CARTESIAN_POINT('',(69.4311098529005,58.5,28.2372649179815));
#18873=CARTESIAN_POINT('',(70.8744855258745,56.5,25.7372649179816));
#18874=CARTESIAN_POINT('',(69.4311098529005,56.5,28.2372649179815));
#18875=CARTESIAN_POINT('',(70.8744855258745,58.5,25.7372649179816));
#18876=CARTESIAN_POINT('Origin',(69.4311098529005,58.5,23.2372649179816));
#18877=CARTESIAN_POINT('',(69.4311098529005,58.5,23.2372649179816));
#18878=CARTESIAN_POINT('',(70.8744855258745,58.5,25.7372649179816));
#18879=CARTESIAN_POINT('',(69.4311098529005,56.5,23.2372649179816));
#18880=CARTESIAN_POINT('',(70.8744855258745,56.5,25.7372649179816));
#18881=CARTESIAN_POINT('',(69.4311098529005,58.5,23.2372649179816));
#18882=CARTESIAN_POINT('Origin',(66.5443585069524,58.5,23.2372649179816));
#18883=CARTESIAN_POINT('',(69.4311098529005,58.5,23.2372649179816));
#18884=CARTESIAN_POINT('',(69.4311098529005,56.5,23.2372649179816));
#18885=CARTESIAN_POINT('Origin',(67.9877341799264,58.5,25.7372649179816));
#18886=CARTESIAN_POINT('Origin',(67.9877341799264,56.5,25.7372649179816));
#18887=CARTESIAN_POINT('',(0.,0.,0.));
#18888=CARTESIAN_POINT('Origin',(384.,29.4811336906747,27.5456750096756));
#18889=CARTESIAN_POINT('',(384.,29.8952421751416,29.8877073880428));
#18890=CARTESIAN_POINT('',(384.,29.4811336906747,27.5456750096756));
#18891=CARTESIAN_POINT('',(384.,29.8952421751416,29.8877073880428));
#18892=CARTESIAN_POINT('',(47.9470000000001,29.4811336906747,27.5456750096756));
#18893=CARTESIAN_POINT('',(384.,29.4811336906747,27.5456750096756));
#18894=CARTESIAN_POINT('',(47.9470000000001,29.8952421751416,29.8877073880428));
#18895=CARTESIAN_POINT('',(47.9470000000001,29.8952421751416,29.8877073880428));
#18896=CARTESIAN_POINT('',(384.,29.8952421751416,29.8877073880428));
#18897=CARTESIAN_POINT('Origin',(384.,30.465859005635,27.3715599497981));
#18898=CARTESIAN_POINT('',(384.,29.643945736254,26.8019472940264));
#18899=CARTESIAN_POINT('Origin',(384.,30.465859005635,27.3715599497981));
#18900=CARTESIAN_POINT('',(47.9470000000001,29.643945736254,26.8019472940264));
#18901=CARTESIAN_POINT('',(384.,29.643945736254,26.8019472940264));
#18902=CARTESIAN_POINT('Origin',(47.9470000000001,30.465859005635,27.3715599497981));
#18903=CARTESIAN_POINT('Origin',(384.,31.5857864376269,24.));
#18904=CARTESIAN_POINT('',(384.,31.5857864376269,24.));
#18905=CARTESIAN_POINT('',(384.,29.643945736254,26.8019472940264));
#18906=CARTESIAN_POINT('',(47.9470000000001,31.5857864376269,24.));
#18907=CARTESIAN_POINT('',(384.,31.5857864376269,24.));
#18908=CARTESIAN_POINT('',(47.9470000000001,29.643945736254,26.8019472940264));
#18909=CARTESIAN_POINT('Origin',(384.,28.8220324668729,26.2323346382546));
#18910=CARTESIAN_POINT('',(384.,28.8220324668729,26.2323346382546));
#18911=CARTESIAN_POINT('',(384.,30.369113052182,24.));
#18912=CARTESIAN_POINT('',(384.,28.8220324668729,26.2323346382546));
#18913=CARTESIAN_POINT('',(47.9470000000001,28.8220324668729,26.2323346382546));
#18914=CARTESIAN_POINT('',(384.,28.8220324668729,26.2323346382546));
#18915=CARTESIAN_POINT('',(47.9470000000001,30.369113052182,24.));
#18916=CARTESIAN_POINT('',(47.9470000000001,28.8220324668729,26.2323346382546));
#18917=CARTESIAN_POINT('',(384.,30.369113052182,24.));
#18918=CARTESIAN_POINT('Origin',(384.,30.465859005635,27.3715599497981));
#18919=CARTESIAN_POINT('',(384.,28.4964083757143,27.7197900695531));
#18920=CARTESIAN_POINT('Origin',(384.,30.465859005635,27.3715599497981));
#18921=CARTESIAN_POINT('',(47.9470000000001,28.4964083757143,27.7197900695531));
#18922=CARTESIAN_POINT('',(384.,28.4964083757143,27.7197900695531));
#18923=CARTESIAN_POINT('Origin',(47.9470000000001,30.465859005635,27.3715599497981));
#18924=CARTESIAN_POINT('Origin',(384.,28.7029146884407,28.8877073880428));
#18925=CARTESIAN_POINT('',(384.,28.7029146884407,28.8877073880428));
#18926=CARTESIAN_POINT('',(384.,28.7029146884407,28.8877073880428));
#18927=CARTESIAN_POINT('',(47.9470000000001,28.7029146884407,28.8877073880428));
#18928=CARTESIAN_POINT('',(384.,28.7029146884407,28.8877073880428));
#18929=CARTESIAN_POINT('',(47.9470000000001,28.7029146884407,28.8877073880428));
#18930=CARTESIAN_POINT('Origin',(384.,28.2105520309605,28.9747649179816));
#18931=CARTESIAN_POINT('',(384.,28.2105520309605,29.4747649179816));
#18932=CARTESIAN_POINT('Origin',(384.,28.2105520309605,28.9747649179816));
#18933=CARTESIAN_POINT('',(47.9470000000001,28.2105520309605,29.4747649179816));
#18934=CARTESIAN_POINT('',(384.,28.2105520309605,29.4747649179816));
#18935=CARTESIAN_POINT('Origin',(47.9470000000001,28.2105520309605,28.9747649179816));
#18936=CARTESIAN_POINT('Origin',(384.,29.4028795176614,29.9747649179816));
#18937=CARTESIAN_POINT('',(384.,29.4028795176614,30.4747649179816));
#18938=CARTESIAN_POINT('Origin',(384.,29.4028795176614,29.9747649179816));
#18939=CARTESIAN_POINT('',(47.9470000000001,29.4028795176614,30.4747649179816));
#18940=CARTESIAN_POINT('Origin',(47.9470000000001,29.4028795176614,29.9747649179816));
#18941=CARTESIAN_POINT('',(384.,29.4028795176614,30.4747649179816));
#18942=CARTESIAN_POINT('Origin',(384.,25.0009567389882,29.4747649179816));
#18943=CARTESIAN_POINT('',(384.,21.7894479690395,29.4747649179816));
#18944=CARTESIAN_POINT('',(384.,25.0009567389882,29.4747649179816));
#18945=CARTESIAN_POINT('',(47.9470000000001,21.7894479690395,29.4747649179816));
#18946=CARTESIAN_POINT('',(384.,21.7894479690395,29.4747649179816));
#18947=CARTESIAN_POINT('',(47.9470000000001,24.9990432610118,29.4747649179816));
#18948=CARTESIAN_POINT('Origin',(384.,20.5188663093253,27.5456750096756));
#18949=CARTESIAN_POINT('',(384.,20.1047578248584,29.8877073880428));
#18950=CARTESIAN_POINT('',(384.,20.5188663093253,27.5456750096756));
#18951=CARTESIAN_POINT('',(384.,20.1047578248584,29.8877073880428));
#18952=CARTESIAN_POINT('',(47.9470000000001,20.1047578248584,29.8877073880428));
#18953=CARTESIAN_POINT('',(384.,20.1047578248584,29.8877073880428));
#18954=CARTESIAN_POINT('',(47.9470000000001,20.5188663093253,27.5456750096756));
#18955=CARTESIAN_POINT('',(47.9470000000001,20.1047578248584,29.8877073880428));
#18956=CARTESIAN_POINT('',(384.,20.5188663093253,27.5456750096756));
#18957=CARTESIAN_POINT('Origin',(384.,19.534140994365,27.3715599497981));
#18958=CARTESIAN_POINT('',(384.,20.356054263746,26.8019472940264));
#18959=CARTESIAN_POINT('Origin',(384.,19.534140994365,27.3715599497981));
#18960=CARTESIAN_POINT('',(47.9470000000001,20.356054263746,26.8019472940264));
#18961=CARTESIAN_POINT('Origin',(47.9470000000001,19.534140994365,27.3715599497981));
#18962=CARTESIAN_POINT('',(384.,20.356054263746,26.8019472940264));
#18963=CARTESIAN_POINT('Origin',(384.,18.4142135623731,24.));
#18964=CARTESIAN_POINT('',(384.,18.4142135623731,24.));
#18965=CARTESIAN_POINT('',(384.,20.356054263746,26.8019472940264));
#18966=CARTESIAN_POINT('',(47.9470000000001,18.4142135623731,24.));
#18967=CARTESIAN_POINT('',(47.9470000000001,20.356054263746,26.8019472940264));
#18968=CARTESIAN_POINT('',(384.,18.4142135623731,24.));
#18969=CARTESIAN_POINT('Origin',(384.,21.1779675331271,26.2323346382546));
#18970=CARTESIAN_POINT('',(384.,21.1779675331271,26.2323346382546));
#18971=CARTESIAN_POINT('',(384.,19.630886947818,24.));
#18972=CARTESIAN_POINT('',(384.,21.1779675331271,26.2323346382546));
#18973=CARTESIAN_POINT('',(47.9470000000001,19.630886947818,24.));
#18974=CARTESIAN_POINT('',(384.,19.630886947818,24.));
#18975=CARTESIAN_POINT('',(47.9470000000001,21.1779675331271,26.2323346382546));
#18976=CARTESIAN_POINT('',(47.9470000000001,21.1779675331271,26.2323346382546));
#18977=CARTESIAN_POINT('',(384.,21.1779675331271,26.2323346382546));
#18978=CARTESIAN_POINT('Origin',(384.,19.534140994365,27.3715599497981));
#18979=CARTESIAN_POINT('',(384.,21.5035916242857,27.7197900695531));
#18980=CARTESIAN_POINT('Origin',(384.,19.534140994365,27.3715599497981));
#18981=CARTESIAN_POINT('',(47.9470000000001,21.5035916242857,27.7197900695531));
#18982=CARTESIAN_POINT('Origin',(47.9470000000001,19.534140994365,27.3715599497981));
#18983=CARTESIAN_POINT('',(384.,21.5035916242857,27.7197900695531));
#18984=CARTESIAN_POINT('Origin',(384.,21.2970853115593,28.8877073880428));
#18985=CARTESIAN_POINT('',(384.,21.2970853115593,28.8877073880428));
#18986=CARTESIAN_POINT('',(384.,21.2970853115593,28.8877073880428));
#18987=CARTESIAN_POINT('',(47.9470000000001,21.2970853115593,28.8877073880428));
#18988=CARTESIAN_POINT('',(47.9470000000001,21.2970853115593,28.8877073880428));
#18989=CARTESIAN_POINT('',(384.,21.2970853115593,28.8877073880428));
#18990=CARTESIAN_POINT('Origin',(384.,21.7894479690395,28.9747649179816));
#18991=CARTESIAN_POINT('Origin',(384.,21.7894479690395,28.9747649179816));
#18992=CARTESIAN_POINT('Origin',(47.9470000000001,21.7894479690395,28.9747649179816));
#18993=CARTESIAN_POINT('Origin',(384.,20.5971204823386,30.4747649179816));
#18994=CARTESIAN_POINT('',(47.9470000000001,20.5971204823386,30.4747649179816));
#18995=CARTESIAN_POINT('',(47.9470000000001,25.0009567389882,30.4747649179816));
#18996=CARTESIAN_POINT('',(384.,20.5971204823386,30.4747649179816));
#18997=CARTESIAN_POINT('',(384.,20.5971204823386,30.4747649179816));
#18998=CARTESIAN_POINT('',(384.,25.0009567389882,30.4747649179816));
#18999=CARTESIAN_POINT('Origin',(384.,20.5971204823386,29.9747649179816));
#19000=CARTESIAN_POINT('Origin',(384.,20.5971204823386,29.9747649179816));
#19001=CARTESIAN_POINT('Origin',(47.9470000000001,20.5971204823386,29.9747649179816));
#19002=CARTESIAN_POINT('Origin',(384.,15.8284271247462,24.));
#19003=CARTESIAN_POINT('',(47.9470000000001,15.8284271247462,24.));
#19004=CARTESIAN_POINT('',(47.9470000000001,21.,24.));
#19005=CARTESIAN_POINT('',(384.,15.8284271247462,24.));
#19006=CARTESIAN_POINT('',(384.,15.8284271247462,24.));
#19007=CARTESIAN_POINT('',(384.,21.,24.));
#19008=CARTESIAN_POINT('Origin',(384.,15.8284271247462,24.));
#19009=CARTESIAN_POINT('',(384.,34.1715728752538,24.));
#19010=CARTESIAN_POINT('',(384.,21.,24.));
#19011=CARTESIAN_POINT('',(47.9470000000001,34.1715728752538,24.));
#19012=CARTESIAN_POINT('',(384.,34.1715728752538,24.));
#19013=CARTESIAN_POINT('',(47.9470000000001,21.,24.));
#19014=CARTESIAN_POINT('Origin',(384.,15.8284271247462,24.));
#19015=CARTESIAN_POINT('',(47.9470000000001,21.,24.));
#19016=CARTESIAN_POINT('',(384.,21.,24.));
#19017=CARTESIAN_POINT('Origin',(384.,34.1715728752538,25.));
#19018=CARTESIAN_POINT('',(384.,34.8786796564404,24.2928932188135));
#19019=CARTESIAN_POINT('Origin',(384.,34.1715728752538,25.));
#19020=CARTESIAN_POINT('',(47.9470000000001,34.8786796564404,24.2928932188135));
#19021=CARTESIAN_POINT('',(384.,34.8786796564404,24.2928932188135));
#19022=CARTESIAN_POINT('Origin',(47.9470000000001,34.1715728752538,25.));
#19023=CARTESIAN_POINT('Origin',(384.,37.3825273013137,26.7967408636868));
#19024=CARTESIAN_POINT('',(384.,37.3825273013137,26.7967408636868));
#19025=CARTESIAN_POINT('',(384.,34.8786796564404,24.2928932188135));
#19026=CARTESIAN_POINT('',(47.9470000000001,37.3825273013137,26.7967408636868));
#19027=CARTESIAN_POINT('',(384.,37.3825273013137,26.7967408636868));
#19028=CARTESIAN_POINT('',(47.9470000000001,34.8786796564404,24.2928932188135));
#19029=CARTESIAN_POINT('Origin',(384.,36.6754205201272,27.5038476448734));
#19030=CARTESIAN_POINT('',(384.,37.6602282731394,27.3301994672064));
#19031=CARTESIAN_POINT('Origin',(384.,36.6754205201272,27.5038476448734));
#19032=CARTESIAN_POINT('',(47.9470000000001,37.6602282731394,27.3301994672064));
#19033=CARTESIAN_POINT('',(384.,37.6602282731394,27.3301994672064));
#19034=CARTESIAN_POINT('Origin',(47.9470000000001,36.6754205201272,27.5038476448734));
#19035=CARTESIAN_POINT('Origin',(384.,38.2147000047147,30.4747649179816));
#19036=CARTESIAN_POINT('',(384.,38.2147000047147,30.4747649179816));
#19037=CARTESIAN_POINT('',(384.,37.6602282731394,27.3301994672064));
#19038=CARTESIAN_POINT('',(47.9470000000001,38.2147000047147,30.4747649179816));
#19039=CARTESIAN_POINT('',(384.,38.2147000047147,30.4747649179816));
#19040=CARTESIAN_POINT('',(47.9470000000001,37.6602282731394,27.3301994672064));
#19041=CARTESIAN_POINT('Origin',(384.,39.2301266166005,30.4747649179816));
#19042=CARTESIAN_POINT('',(384.,39.2301266166005,30.4747649179816));
#19043=CARTESIAN_POINT('',(384.,39.2301266166005,30.4747649179816));
#19044=CARTESIAN_POINT('',(47.9470000000001,39.2301266166005,30.4747649179816));
#19045=CARTESIAN_POINT('',(384.,39.2301266166005,30.4747649179816));
#19046=CARTESIAN_POINT('',(47.9470000000001,39.2301266166005,30.4747649179816));
#19047=CARTESIAN_POINT('Origin',(384.,38.6450360261516,27.1565512895395));
#19048=CARTESIAN_POINT('',(384.,38.6450360261516,27.1565512895395));
#19049=CARTESIAN_POINT('',(384.,38.6450360261516,27.1565512895395));
#19050=CARTESIAN_POINT('',(47.9470000000001,38.6450360261516,27.1565512895395));
#19051=CARTESIAN_POINT('',(384.,38.6450360261516,27.1565512895395));
#19052=CARTESIAN_POINT('',(47.9470000000001,38.6450360261516,27.1565512895395));
#19053=CARTESIAN_POINT('Origin',(384.,36.6754205201272,27.5038476448734));
#19054=CARTESIAN_POINT('',(384.,38.0896340825003,26.0896340825003));
#19055=CARTESIAN_POINT('Origin',(384.,36.6754205201272,27.5038476448734));
#19056=CARTESIAN_POINT('',(47.9470000000001,38.0896340825003,26.0896340825003));
#19057=CARTESIAN_POINT('',(384.,38.0896340825003,26.0896340825003));
#19058=CARTESIAN_POINT('Origin',(47.9470000000001,36.6754205201272,27.5038476448734));
#19059=CARTESIAN_POINT('Origin',(384.,35.5857864376269,23.5857864376269));
#19060=CARTESIAN_POINT('',(384.,35.5857864376269,23.5857864376269));
#19061=CARTESIAN_POINT('',(384.,35.5857864376269,23.5857864376269));
#19062=CARTESIAN_POINT('',(47.9470000000001,35.5857864376269,23.5857864376269));
#19063=CARTESIAN_POINT('',(384.,35.5857864376269,23.5857864376269));
#19064=CARTESIAN_POINT('',(47.9470000000001,35.5857864376269,23.5857864376269));
#19065=CARTESIAN_POINT('Origin',(384.,34.1715728752538,25.));
#19066=CARTESIAN_POINT('',(384.,34.1715728752538,23.));
#19067=CARTESIAN_POINT('Origin',(384.,34.1715728752538,25.));
#19068=CARTESIAN_POINT('',(47.9470000000001,34.1715728752538,23.));
#19069=CARTESIAN_POINT('',(384.,34.1715728752538,23.));
#19070=CARTESIAN_POINT('Origin',(47.9470000000001,34.1715728752538,25.));
#19071=CARTESIAN_POINT('Origin',(384.,25.,23.));
#19072=CARTESIAN_POINT('',(384.,15.8284271247462,23.));
#19073=CARTESIAN_POINT('',(384.,25.,23.));
#19074=CARTESIAN_POINT('',(47.9470000000001,15.8284271247462,23.));
#19075=CARTESIAN_POINT('',(384.,15.8284271247462,23.));
#19076=CARTESIAN_POINT('',(47.9470000000001,25.,23.));
#19077=CARTESIAN_POINT('Origin',(384.,15.8284271247462,25.));
#19078=CARTESIAN_POINT('',(384.,15.1213203435596,24.2928932188135));
#19079=CARTESIAN_POINT('Origin',(384.,15.8284271247462,25.));
#19080=CARTESIAN_POINT('',(47.9470000000001,15.1213203435596,24.2928932188135));
#19081=CARTESIAN_POINT('Origin',(47.9470000000001,15.8284271247462,25.));
#19082=CARTESIAN_POINT('',(384.,15.1213203435596,24.2928932188135));
#19083=CARTESIAN_POINT('Origin',(384.,12.6174726986863,26.7967408636868));
#19084=CARTESIAN_POINT('',(384.,12.6174726986863,26.7967408636868));
#19085=CARTESIAN_POINT('',(384.,15.1213203435596,24.2928932188135));
#19086=CARTESIAN_POINT('',(47.9470000000001,12.6174726986863,26.7967408636868));
#19087=CARTESIAN_POINT('',(47.9470000000001,15.1213203435596,24.2928932188135));
#19088=CARTESIAN_POINT('',(384.,12.6174726986863,26.7967408636868));
#19089=CARTESIAN_POINT('Origin',(384.,13.3245794798728,27.5038476448734));
#19090=CARTESIAN_POINT('',(384.,12.3397717268606,27.3301994672064));
#19091=CARTESIAN_POINT('Origin',(384.,13.3245794798728,27.5038476448734));
#19092=CARTESIAN_POINT('',(47.9470000000001,12.3397717268606,27.3301994672064));
#19093=CARTESIAN_POINT('Origin',(47.9470000000001,13.3245794798728,27.5038476448734));
#19094=CARTESIAN_POINT('',(384.,12.3397717268606,27.3301994672064));
#19095=CARTESIAN_POINT('Origin',(384.,11.7852999952853,30.4747649179816));
#19096=CARTESIAN_POINT('',(384.,11.7852999952853,30.4747649179816));
#19097=CARTESIAN_POINT('',(384.,12.3397717268606,27.3301994672064));
#19098=CARTESIAN_POINT('',(47.9470000000001,11.7852999952853,30.4747649179816));
#19099=CARTESIAN_POINT('',(47.9470000000001,12.3397717268606,27.3301994672064));
#19100=CARTESIAN_POINT('',(384.,11.7852999952853,30.4747649179816));
#19101=CARTESIAN_POINT('Origin',(384.,10.7698733833995,30.4747649179816));
#19102=CARTESIAN_POINT('',(384.,10.7698733833995,30.4747649179816));
#19103=CARTESIAN_POINT('',(384.,10.7698733833995,30.4747649179816));
#19104=CARTESIAN_POINT('',(47.9470000000001,10.7698733833995,30.4747649179816));
#19105=CARTESIAN_POINT('',(47.9470000000001,10.7698733833995,30.4747649179816));
#19106=CARTESIAN_POINT('',(384.,10.7698733833995,30.4747649179816));
#19107=CARTESIAN_POINT('Origin',(384.,11.3549639738484,27.1565512895395));
#19108=CARTESIAN_POINT('',(384.,11.3549639738484,27.1565512895395));
#19109=CARTESIAN_POINT('',(384.,11.3549639738484,27.1565512895395));
#19110=CARTESIAN_POINT('',(47.9470000000001,11.3549639738484,27.1565512895395));
#19111=CARTESIAN_POINT('',(47.9470000000001,11.3549639738484,27.1565512895395));
#19112=CARTESIAN_POINT('',(384.,11.3549639738484,27.1565512895395));
#19113=CARTESIAN_POINT('Origin',(384.,13.3245794798728,27.5038476448734));
#19114=CARTESIAN_POINT('',(384.,11.9103659174997,26.0896340825003));
#19115=CARTESIAN_POINT('Origin',(384.,13.3245794798728,27.5038476448734));
#19116=CARTESIAN_POINT('',(47.9470000000001,11.9103659174997,26.0896340825003));
#19117=CARTESIAN_POINT('Origin',(47.9470000000001,13.3245794798728,27.5038476448734));
#19118=CARTESIAN_POINT('',(384.,11.9103659174997,26.0896340825003));
#19119=CARTESIAN_POINT('Origin',(384.,14.4142135623731,23.5857864376269));
#19120=CARTESIAN_POINT('',(384.,14.4142135623731,23.5857864376269));
#19121=CARTESIAN_POINT('',(384.,14.4142135623731,23.5857864376269));
#19122=CARTESIAN_POINT('',(47.9470000000001,14.4142135623731,23.5857864376269));
#19123=CARTESIAN_POINT('',(47.9470000000001,14.4142135623731,23.5857864376269));
#19124=CARTESIAN_POINT('',(384.,14.4142135623731,23.5857864376269));
#19125=CARTESIAN_POINT('Origin',(384.,15.8284271247462,25.));
#19126=CARTESIAN_POINT('Origin',(384.,15.8284271247462,25.));
#19127=CARTESIAN_POINT('Origin',(47.9470000000001,15.8284271247462,25.));
#19128=CARTESIAN_POINT('Origin',(384.,17.8849366916998,26.7373824589908));
#19129=CARTESIAN_POINT('Origin',(47.9470000000001,17.8849366916998,26.7373824589908));
#19130=CARTESIAN_POINT('',(0.,0.,0.));
#19131=CARTESIAN_POINT('Origin',(67.9877341799264,62.5,25.7372649179816));
#19132=CARTESIAN_POINT('',(69.4527341799265,60.5,25.7372649179816));
#19133=CARTESIAN_POINT('Origin',(67.9877341799264,60.5,25.7372649179816));
#19134=CARTESIAN_POINT('',(69.4527341799265,62.5,25.7372649179816));
#19135=CARTESIAN_POINT('',(69.4527341799264,62.5,25.7372649179816));
#19136=CARTESIAN_POINT('Origin',(67.9877341799264,62.5,25.7372649179816));
#19137=CARTESIAN_POINT('Origin',(65.1009828339783,62.5,25.7372649179816));
#19138=CARTESIAN_POINT('',(66.5443585069524,62.5,23.2372649179816));
#19139=CARTESIAN_POINT('',(65.1009828339783,62.5,25.7372649179816));
#19140=CARTESIAN_POINT('',(66.5443585069524,62.5,23.2372649179816));
#19141=CARTESIAN_POINT('',(66.5443585069524,60.5,23.2372649179816));
#19142=CARTESIAN_POINT('',(66.5443585069524,62.5,23.2372649179816));
#19143=CARTESIAN_POINT('',(65.1009828339783,60.5,25.7372649179816));
#19144=CARTESIAN_POINT('',(66.5443585069524,60.5,23.2372649179816));
#19145=CARTESIAN_POINT('',(65.1009828339783,62.5,25.7372649179816));
#19146=CARTESIAN_POINT('Origin',(66.5443585069524,62.5,28.2372649179815));
#19147=CARTESIAN_POINT('',(66.5443585069524,62.5,28.2372649179815));
#19148=CARTESIAN_POINT('',(65.1009828339783,62.5,25.7372649179816));
#19149=CARTESIAN_POINT('',(66.5443585069524,60.5,28.2372649179815));
#19150=CARTESIAN_POINT('',(65.1009828339783,60.5,25.7372649179816));
#19151=CARTESIAN_POINT('',(66.5443585069524,62.5,28.2372649179815));
#19152=CARTESIAN_POINT('Origin',(69.4311098529005,62.5,28.2372649179815));
#19153=CARTESIAN_POINT('',(69.4311098529005,62.5,28.2372649179815));
#19154=CARTESIAN_POINT('',(66.5443585069524,62.5,28.2372649179815));
#19155=CARTESIAN_POINT('',(69.4311098529005,60.5,28.2372649179815));
#19156=CARTESIAN_POINT('',(66.5443585069524,60.5,28.2372649179815));
#19157=CARTESIAN_POINT('',(69.4311098529005,62.5,28.2372649179815));
#19158=CARTESIAN_POINT('Origin',(70.8744855258745,62.5,25.7372649179816));
#19159=CARTESIAN_POINT('',(70.8744855258745,62.5,25.7372649179816));
#19160=CARTESIAN_POINT('',(69.4311098529005,62.5,28.2372649179815));
#19161=CARTESIAN_POINT('',(70.8744855258745,60.5,25.7372649179816));
#19162=CARTESIAN_POINT('',(69.4311098529005,60.5,28.2372649179815));
#19163=CARTESIAN_POINT('',(70.8744855258745,62.5,25.7372649179816));
#19164=CARTESIAN_POINT('Origin',(69.4311098529005,62.5,23.2372649179816));
#19165=CARTESIAN_POINT('',(69.4311098529005,62.5,23.2372649179816));
#19166=CARTESIAN_POINT('',(70.8744855258745,62.5,25.7372649179816));
#19167=CARTESIAN_POINT('',(69.4311098529005,60.5,23.2372649179816));
#19168=CARTESIAN_POINT('',(70.8744855258745,60.5,25.7372649179816));
#19169=CARTESIAN_POINT('',(69.4311098529005,62.5,23.2372649179816));
#19170=CARTESIAN_POINT('Origin',(66.5443585069524,62.5,23.2372649179816));
#19171=CARTESIAN_POINT('',(69.4311098529005,62.5,23.2372649179816));
#19172=CARTESIAN_POINT('',(69.4311098529005,60.5,23.2372649179816));
#19173=CARTESIAN_POINT('Origin',(67.9877341799264,62.5,25.7372649179816));
#19174=CARTESIAN_POINT('Origin',(67.9877341799264,60.5,25.7372649179816));
#19175=CARTESIAN_POINT('',(0.,0.,0.));
#19176=CARTESIAN_POINT('',(0.,0.,0.));
#19177=CARTESIAN_POINT('',(0.,0.,0.));
#19178=CARTESIAN_POINT('',(0.,0.,0.));
#19179=CARTESIAN_POINT('',(0.,0.,0.));
#19180=CARTESIAN_POINT('',(0.,0.,0.));
#19181=CARTESIAN_POINT('',(0.,0.,0.));
#19182=CARTESIAN_POINT('',(0.,0.,0.));
#19183=CARTESIAN_POINT('',(0.,0.,0.));
#19184=CARTESIAN_POINT('',(0.,0.,0.));
#19185=CARTESIAN_POINT('',(0.,0.,0.));
#19186=CARTESIAN_POINT('',(0.,0.,0.));
#19187=CARTESIAN_POINT('',(0.,0.,0.));
#19188=CARTESIAN_POINT('',(0.,0.,0.));
#19189=UNCERTAINTY_MEASURE_WITH_UNIT(LENGTH_MEASURE(0.01),#19221,
'DISTANCE_ACCURACY_VALUE',
'Maximum model space distance between geometric entities at asserted c
onnectivities');
#19190=UNCERTAINTY_MEASURE_WITH_UNIT(LENGTH_MEASURE(0.01),#19221,
'DISTANCE_ACCURACY_VALUE',
'Maximum model space distance between geometric entities at asserted c
onnectivities');
#19191=UNCERTAINTY_MEASURE_WITH_UNIT(LENGTH_MEASURE(0.01),#19221,
'DISTANCE_ACCURACY_VALUE',
'Maximum model space distance between geometric entities at asserted c
onnectivities');
#19192=UNCERTAINTY_MEASURE_WITH_UNIT(LENGTH_MEASURE(0.01),#19221,
'DISTANCE_ACCURACY_VALUE',
'Maximum model space distance between geometric entities at asserted c
onnectivities');
#19193=UNCERTAINTY_MEASURE_WITH_UNIT(LENGTH_MEASURE(0.01),#19221,
'DISTANCE_ACCURACY_VALUE',
'Maximum model space distance between geometric entities at asserted c
onnectivities');
#19194=UNCERTAINTY_MEASURE_WITH_UNIT(LENGTH_MEASURE(0.01),#19221,
'DISTANCE_ACCURACY_VALUE',
'Maximum model space distance between geometric entities at asserted c
onnectivities');
#19195=UNCERTAINTY_MEASURE_WITH_UNIT(LENGTH_MEASURE(0.01),#19221,
'DISTANCE_ACCURACY_VALUE',
'Maximum model space distance between geometric entities at asserted c
onnectivities');
#19196=UNCERTAINTY_MEASURE_WITH_UNIT(LENGTH_MEASURE(0.01),#19221,
'DISTANCE_ACCURACY_VALUE',
'Maximum model space distance between geometric entities at asserted c
onnectivities');
#19197=UNCERTAINTY_MEASURE_WITH_UNIT(LENGTH_MEASURE(0.01),#19221,
'DISTANCE_ACCURACY_VALUE',
'Maximum model space distance between geometric entities at asserted c
onnectivities');
#19198=UNCERTAINTY_MEASURE_WITH_UNIT(LENGTH_MEASURE(0.01),#19221,
'DISTANCE_ACCURACY_VALUE',
'Maximum model space distance between geometric entities at asserted c
onnectivities');
#19199=UNCERTAINTY_MEASURE_WITH_UNIT(LENGTH_MEASURE(0.01),#19221,
'DISTANCE_ACCURACY_VALUE',
'Maximum model space distance between geometric entities at asserted c
onnectivities');
#19200=UNCERTAINTY_MEASURE_WITH_UNIT(LENGTH_MEASURE(0.01),#19221,
'DISTANCE_ACCURACY_VALUE',
'Maximum model space distance between geometric entities at asserted c
onnectivities');
#19201=UNCERTAINTY_MEASURE_WITH_UNIT(LENGTH_MEASURE(0.01),#19221,
'DISTANCE_ACCURACY_VALUE',
'Maximum model space distance between geometric entities at asserted c
onnectivities');
#19202=UNCERTAINTY_MEASURE_WITH_UNIT(LENGTH_MEASURE(0.01),#19221,
'DISTANCE_ACCURACY_VALUE',
'Maximum model space distance between geometric entities at asserted c
onnectivities');
#19203=UNCERTAINTY_MEASURE_WITH_UNIT(LENGTH_MEASURE(0.01),#19221,
'DISTANCE_ACCURACY_VALUE',
'Maximum model space distance between geometric entities at asserted c
onnectivities');
#19204=UNCERTAINTY_MEASURE_WITH_UNIT(LENGTH_MEASURE(0.01),#19221,
'DISTANCE_ACCURACY_VALUE',
'Maximum model space distance between geometric entities at asserted c
onnectivities');
#19205=(
GEOMETRIC_REPRESENTATION_CONTEXT(3)
GLOBAL_UNCERTAINTY_ASSIGNED_CONTEXT((#19189))
GLOBAL_UNIT_ASSIGNED_CONTEXT((#19221,#19223,#19224))
REPRESENTATION_CONTEXT('','3D')
);
#19206=(
GEOMETRIC_REPRESENTATION_CONTEXT(3)
GLOBAL_UNCERTAINTY_ASSIGNED_CONTEXT((#19190))
GLOBAL_UNIT_ASSIGNED_CONTEXT((#19221,#19223,#19224))
REPRESENTATION_CONTEXT('','3D')
);
#19207=(
GEOMETRIC_REPRESENTATION_CONTEXT(3)
GLOBAL_UNCERTAINTY_ASSIGNED_CONTEXT((#19191))
GLOBAL_UNIT_ASSIGNED_CONTEXT((#19221,#19223,#19224))
REPRESENTATION_CONTEXT('','3D')
);
#19208=(
GEOMETRIC_REPRESENTATION_CONTEXT(3)
GLOBAL_UNCERTAINTY_ASSIGNED_CONTEXT((#19192))
GLOBAL_UNIT_ASSIGNED_CONTEXT((#19221,#19223,#19224))
REPRESENTATION_CONTEXT('','3D')
);
#19209=(
GEOMETRIC_REPRESENTATION_CONTEXT(3)
GLOBAL_UNCERTAINTY_ASSIGNED_CONTEXT((#19193))
GLOBAL_UNIT_ASSIGNED_CONTEXT((#19221,#19223,#19224))
REPRESENTATION_CONTEXT('','3D')
);
#19210=(
GEOMETRIC_REPRESENTATION_CONTEXT(3)
GLOBAL_UNCERTAINTY_ASSIGNED_CONTEXT((#19194))
GLOBAL_UNIT_ASSIGNED_CONTEXT((#19221,#19223,#19224))
REPRESENTATION_CONTEXT('','3D')
);
#19211=(
GEOMETRIC_REPRESENTATION_CONTEXT(3)
GLOBAL_UNCERTAINTY_ASSIGNED_CONTEXT((#19195))
GLOBAL_UNIT_ASSIGNED_CONTEXT((#19221,#19223,#19224))
REPRESENTATION_CONTEXT('','3D')
);
#19212=(
GEOMETRIC_REPRESENTATION_CONTEXT(3)
GLOBAL_UNCERTAINTY_ASSIGNED_CONTEXT((#19196))
GLOBAL_UNIT_ASSIGNED_CONTEXT((#19221,#19223,#19224))
REPRESENTATION_CONTEXT('','3D')
);
#19213=(
GEOMETRIC_REPRESENTATION_CONTEXT(3)
GLOBAL_UNCERTAINTY_ASSIGNED_CONTEXT((#19197))
GLOBAL_UNIT_ASSIGNED_CONTEXT((#19221,#19223,#19224))
REPRESENTATION_CONTEXT('','3D')
);
#19214=(
GEOMETRIC_REPRESENTATION_CONTEXT(3)
GLOBAL_UNCERTAINTY_ASSIGNED_CONTEXT((#19198))
GLOBAL_UNIT_ASSIGNED_CONTEXT((#19221,#19223,#19224))
REPRESENTATION_CONTEXT('','3D')
);
#19215=(
GEOMETRIC_REPRESENTATION_CONTEXT(3)
GLOBAL_UNCERTAINTY_ASSIGNED_CONTEXT((#19199))
GLOBAL_UNIT_ASSIGNED_CONTEXT((#19221,#19223,#19224))
REPRESENTATION_CONTEXT('','3D')
);
#19216=(
GEOMETRIC_REPRESENTATION_CONTEXT(3)
GLOBAL_UNCERTAINTY_ASSIGNED_CONTEXT((#19200))
GLOBAL_UNIT_ASSIGNED_CONTEXT((#19221,#19223,#19224))
REPRESENTATION_CONTEXT('','3D')
);
#19217=(
GEOMETRIC_REPRESENTATION_CONTEXT(3)
GLOBAL_UNCERTAINTY_ASSIGNED_CONTEXT((#19201))
GLOBAL_UNIT_ASSIGNED_CONTEXT((#19221,#19223,#19224))
REPRESENTATION_CONTEXT('','3D')
);
#19218=(
GEOMETRIC_REPRESENTATION_CONTEXT(3)
GLOBAL_UNCERTAINTY_ASSIGNED_CONTEXT((#19202))
GLOBAL_UNIT_ASSIGNED_CONTEXT((#19221,#19223,#19224))
REPRESENTATION_CONTEXT('','3D')
);
#19219=(
GEOMETRIC_REPRESENTATION_CONTEXT(3)
GLOBAL_UNCERTAINTY_ASSIGNED_CONTEXT((#19203))
GLOBAL_UNIT_ASSIGNED_CONTEXT((#19221,#19223,#19224))
REPRESENTATION_CONTEXT('','3D')
);
#19220=(
GEOMETRIC_REPRESENTATION_CONTEXT(3)
GLOBAL_UNCERTAINTY_ASSIGNED_CONTEXT((#19204))
GLOBAL_UNIT_ASSIGNED_CONTEXT((#19221,#19223,#19224))
REPRESENTATION_CONTEXT('','3D')
);
#19221=(
LENGTH_UNIT()
NAMED_UNIT(*)
SI_UNIT(.MILLI.,.METRE.)
);
#19222=(
LENGTH_UNIT()
NAMED_UNIT(*)
SI_UNIT($,.METRE.)
);
#19223=(
NAMED_UNIT(*)
PLANE_ANGLE_UNIT()
SI_UNIT($,.RADIAN.)
);
#19224=(
NAMED_UNIT(*)
SI_UNIT($,.STERADIAN.)
SOLID_ANGLE_UNIT()
);
#19225=SHAPE_DEFINITION_REPRESENTATION(#19240,#19269);
#19226=SHAPE_DEFINITION_REPRESENTATION(#19241,#19270);
#19227=SHAPE_DEFINITION_REPRESENTATION(#19242,#19271);
#19228=SHAPE_DEFINITION_REPRESENTATION(#19243,#19272);
#19229=SHAPE_DEFINITION_REPRESENTATION(#19244,#19273);
#19230=SHAPE_DEFINITION_REPRESENTATION(#19245,#19274);
#19231=SHAPE_DEFINITION_REPRESENTATION(#19246,#19275);
#19232=SHAPE_DEFINITION_REPRESENTATION(#19247,#19276);
#19233=SHAPE_DEFINITION_REPRESENTATION(#19248,#19277);
#19234=SHAPE_DEFINITION_REPRESENTATION(#19249,#19278);
#19235=SHAPE_DEFINITION_REPRESENTATION(#19250,#19279);
#19236=SHAPE_DEFINITION_REPRESENTATION(#19251,#19280);
#19237=SHAPE_DEFINITION_REPRESENTATION(#19252,#19281);
#19238=SHAPE_DEFINITION_REPRESENTATION(#19253,#19282);
#19239=SHAPE_DEFINITION_REPRESENTATION(#19254,#19283);
#19240=PRODUCT_DEFINITION_SHAPE('',$,#19285);
#19241=PRODUCT_DEFINITION_SHAPE('',$,#19286);
#19242=PRODUCT_DEFINITION_SHAPE('',$,#19287);
#19243=PRODUCT_DEFINITION_SHAPE('',$,#19288);
#19244=PRODUCT_DEFINITION_SHAPE('',$,#19289);
#19245=PRODUCT_DEFINITION_SHAPE('',$,#19290);
#19246=PRODUCT_DEFINITION_SHAPE('',$,#19291);
#19247=PRODUCT_DEFINITION_SHAPE('',$,#19292);
#19248=PRODUCT_DEFINITION_SHAPE('',$,#19293);
#19249=PRODUCT_DEFINITION_SHAPE('',$,#19294);
#19250=PRODUCT_DEFINITION_SHAPE('',$,#19295);
#19251=PRODUCT_DEFINITION_SHAPE('',$,#19296);
#19252=PRODUCT_DEFINITION_SHAPE('',$,#19297);
#19253=PRODUCT_DEFINITION_SHAPE('',$,#19298);
#19254=PRODUCT_DEFINITION_SHAPE('',$,#19299);
#19255=PRODUCT_DEFINITION_SHAPE($,$,#53);
#19256=PRODUCT_DEFINITION_SHAPE($,$,#54);
#19257=PRODUCT_DEFINITION_SHAPE($,$,#55);
#19258=PRODUCT_DEFINITION_SHAPE($,$,#56);
#19259=PRODUCT_DEFINITION_SHAPE($,$,#57);
#19260=PRODUCT_DEFINITION_SHAPE($,$,#58);
#19261=PRODUCT_DEFINITION_SHAPE($,$,#59);
#19262=PRODUCT_DEFINITION_SHAPE($,$,#60);
#19263=PRODUCT_DEFINITION_SHAPE($,$,#61);
#19264=PRODUCT_DEFINITION_SHAPE($,$,#62);
#19265=PRODUCT_DEFINITION_SHAPE($,$,#63);
#19266=PRODUCT_DEFINITION_SHAPE($,$,#64);
#19267=PRODUCT_DEFINITION_SHAPE($,$,#65);
#19268=PRODUCT_DEFINITION_SHAPE($,$,#66);
#19269=SHAPE_REPRESENTATION('',(#11483,#12714,#12715,#12716,#12717,#12718,
#12719,#12720,#12721,#12722,#12723,#12724,#12725,#12726,#12727),#19205);
#19270=SHAPE_REPRESENTATION('',(#11484),#19206);
#19271=SHAPE_REPRESENTATION('',(#11522),#19207);
#19272=SHAPE_REPRESENTATION('',(#11555),#19208);
#19273=SHAPE_REPRESENTATION('',(#11671),#19209);
#19274=SHAPE_REPRESENTATION('',(#11684),#19210);
#19275=SHAPE_REPRESENTATION('',(#11759),#19211);
#19276=SHAPE_REPRESENTATION('',(#12374),#19212);
#19277=SHAPE_REPRESENTATION('',(#12476),#19213);
#19278=SHAPE_REPRESENTATION('',(#12488),#19214);
#19279=SHAPE_REPRESENTATION('',(#12590),#19215);
#19280=SHAPE_REPRESENTATION('',(#12603),#19216);
#19281=SHAPE_REPRESENTATION('',(#12615),#19217);
#19282=SHAPE_REPRESENTATION('',(#12627),#19218);
#19283=SHAPE_REPRESENTATION('',(#12702),#19219);
#19284=PRODUCT_DEFINITION_CONTEXT('part definition',#19331,'design');
#19285=PRODUCT_DEFINITION('MAS-275','MAS-275',#19300,#19284);
#19286=PRODUCT_DEFINITION('Motor (1)','Motor (1)',#19301,#19284);
#19287=PRODUCT_DEFINITION('Ring (1)','Ring (1)',#19302,#19284);
#19288=PRODUCT_DEFINITION('Motor_Mount (1)','Motor_Mount (1)',#19303,#19284);
#19289=PRODUCT_DEFINITION('M3_Screw_01 (1)','M3_Screw_01 (1)',#19304,#19284);
#19290=PRODUCT_DEFINITION('Slider_01 (1)','Slider_01 (1)',#19305,#19284);
#19291=PRODUCT_DEFINITION('Base (1)','Base (1)',#19306,#19284);
#19292=PRODUCT_DEFINITION('Bracket_01 (1)','Bracket_01 (1)',#19307,#19284);
#19293=PRODUCT_DEFINITION('M3_Nut_01 (1)','M3_Nut_01 (1)',#19308,#19284);
#19294=PRODUCT_DEFINITION('Bracket_02 (1)','Bracket_02 (1)',#19309,#19284);
#19295=PRODUCT_DEFINITION('M3_Screw_02 (1)','M3_Screw_02 (1)',#19310,#19284);
#19296=PRODUCT_DEFINITION('M3_Nut_02 (1)','M3_Nut_02 (1)',#19311,#19284);
#19297=PRODUCT_DEFINITION('M3_Nut_03 (1)','M3_Nut_03 (1)',#19312,#19284);
#19298=PRODUCT_DEFINITION('Slider_02 (1)','Slider_02 (1)',#19313,#19284);
#19299=PRODUCT_DEFINITION('M3_Nut_04 (1)','M3_Nut_04 (1)',#19314,#19284);
#19300=PRODUCT_DEFINITION_FORMATION('',$,#19333);
#19301=PRODUCT_DEFINITION_FORMATION('',$,#19334);
#19302=PRODUCT_DEFINITION_FORMATION('',$,#19335);
#19303=PRODUCT_DEFINITION_FORMATION('',$,#19336);
#19304=PRODUCT_DEFINITION_FORMATION('',$,#19337);
#19305=PRODUCT_DEFINITION_FORMATION('',$,#19338);
#19306=PRODUCT_DEFINITION_FORMATION('',$,#19339);
#19307=PRODUCT_DEFINITION_FORMATION('',$,#19340);
#19308=PRODUCT_DEFINITION_FORMATION('',$,#19341);
#19309=PRODUCT_DEFINITION_FORMATION('',$,#19342);
#19310=PRODUCT_DEFINITION_FORMATION('',$,#19343);
#19311=PRODUCT_DEFINITION_FORMATION('',$,#19344);
#19312=PRODUCT_DEFINITION_FORMATION('',$,#19345);
#19313=PRODUCT_DEFINITION_FORMATION('',$,#19346);
#19314=PRODUCT_DEFINITION_FORMATION('',$,#19347);
#19315=PRODUCT_RELATED_PRODUCT_CATEGORY('MAS-275','MAS-275',(#19333));
#19316=PRODUCT_RELATED_PRODUCT_CATEGORY('Motor (1)','Motor (1)',(#19334));
#19317=PRODUCT_RELATED_PRODUCT_CATEGORY('Ring (1)','Ring (1)',(#19335));
#19318=PRODUCT_RELATED_PRODUCT_CATEGORY('Motor_Mount (1)',
'Motor_Mount (1)',(#19336));
#19319=PRODUCT_RELATED_PRODUCT_CATEGORY('M3_Screw_01 (1)',
'M3_Screw_01 (1)',(#19337));
#19320=PRODUCT_RELATED_PRODUCT_CATEGORY('Slider_01 (1)','Slider_01 (1)',
(#19338));
#19321=PRODUCT_RELATED_PRODUCT_CATEGORY('Base (1)','Base (1)',(#19339));
#19322=PRODUCT_RELATED_PRODUCT_CATEGORY('Bracket_01 (1)',
'Bracket_01 (1)',(#19340));
#19323=PRODUCT_RELATED_PRODUCT_CATEGORY('M3_Nut_01 (1)','M3_Nut_01 (1)',
(#19341));
#19324=PRODUCT_RELATED_PRODUCT_CATEGORY('Bracket_02 (1)',
'Bracket_02 (1)',(#19342));
#19325=PRODUCT_RELATED_PRODUCT_CATEGORY('M3_Screw_02 (1)',
'M3_Screw_02 (1)',(#19343));
#19326=PRODUCT_RELATED_PRODUCT_CATEGORY('M3_Nut_02 (1)','M3_Nut_02 (1)',
(#19344));
#19327=PRODUCT_RELATED_PRODUCT_CATEGORY('M3_Nut_03 (1)','M3_Nut_03 (1)',
(#19345));
#19328=PRODUCT_RELATED_PRODUCT_CATEGORY('Slider_02 (1)','Slider_02 (1)',
(#19346));
#19329=PRODUCT_RELATED_PRODUCT_CATEGORY('M3_Nut_04 (1)','M3_Nut_04 (1)',
(#19347));
#19330=APPLICATION_PROTOCOL_DEFINITION('international standard',
'automotive_design',2009,#19331);
#19331=APPLICATION_CONTEXT(
'Core Data for Automotive Mechanical Design Process');
#19332=PRODUCT_CONTEXT('part definition',#19331,'mechanical');
#19333=PRODUCT('MAS-275','MAS-275',$,(#19332));
#19334=PRODUCT('Motor (1)','Motor (1)',$,(#19332));
#19335=PRODUCT('Ring (1)','Ring (1)',$,(#19332));
#19336=PRODUCT('Motor_Mount (1)','Motor_Mount (1)',$,(#19332));
#19337=PRODUCT('M3_Screw_01 (1)','M3_Screw_01 (1)',$,(#19332));
#19338=PRODUCT('Slider_01 (1)','Slider_01 (1)',$,(#19332));
#19339=PRODUCT('Base (1)','Base (1)',$,(#19332));
#19340=PRODUCT('Bracket_01 (1)','Bracket_01 (1)',$,(#19332));
#19341=PRODUCT('M3_Nut_01 (1)','M3_Nut_01 (1)',$,(#19332));
#19342=PRODUCT('Bracket_02 (1)','Bracket_02 (1)',$,(#19332));
#19343=PRODUCT('M3_Screw_02 (1)','M3_Screw_02 (1)',$,(#19332));
#19344=PRODUCT('M3_Nut_02 (1)','M3_Nut_02 (1)',$,(#19332));
#19345=PRODUCT('M3_Nut_03 (1)','M3_Nut_03 (1)',$,(#19332));
#19346=PRODUCT('Slider_02 (1)','Slider_02 (1)',$,(#19332));
#19347=PRODUCT('M3_Nut_04 (1)','M3_Nut_04 (1)',$,(#19332));
#19348=PRESENTATION_STYLE_ASSIGNMENT((#19352));
#19349=PRESENTATION_STYLE_ASSIGNMENT((#19353));
#19350=PRESENTATION_STYLE_ASSIGNMENT((#19354));
#19351=PRESENTATION_STYLE_ASSIGNMENT((#19355));
#19352=SURFACE_STYLE_USAGE(.BOTH.,#19356);
#19353=SURFACE_STYLE_USAGE(.BOTH.,#19357);
#19354=SURFACE_STYLE_USAGE(.BOTH.,#19358);
#19355=SURFACE_STYLE_USAGE(.BOTH.,#19359);
#19356=SURFACE_SIDE_STYLE('',(#19360));
#19357=SURFACE_SIDE_STYLE('',(#19361));
#19358=SURFACE_SIDE_STYLE('',(#19362));
#19359=SURFACE_SIDE_STYLE('',(#19363));
#19360=SURFACE_STYLE_FILL_AREA(#19364);
#19361=SURFACE_STYLE_FILL_AREA(#19365);
#19362=SURFACE_STYLE_FILL_AREA(#19366);
#19363=SURFACE_STYLE_FILL_AREA(#19367);
#19364=FILL_AREA_STYLE('Steel - Satin',(#19368));
#19365=FILL_AREA_STYLE('Steel - Satin',(#19369));
#19366=FILL_AREA_STYLE('Steel - Satin (1)',(#19370));
#19367=FILL_AREA_STYLE('Steel - Satin (1) (1)',(#19371));
#19368=FILL_AREA_STYLE_COLOUR('Steel - Satin',#19372);
#19369=FILL_AREA_STYLE_COLOUR('Steel - Satin',#19373);
#19370=FILL_AREA_STYLE_COLOUR('Steel - Satin (1)',#19374);
#19371=FILL_AREA_STYLE_COLOUR('Steel - Satin (1) (1)',#19375);
#19372=COLOUR_RGB('Steel - Satin',0.627450980392157,0.627450980392157,0.627450980392157);
#19373=COLOUR_RGB('Steel - Satin',0.843137254901961,0.843137254901961,0.843137254901961);
#19374=COLOUR_RGB('Steel - Satin (1)',0.356862745098039,0.356862745098039,
0.356862745098039);
#19375=COLOUR_RGB('Steel - Satin (1) (1)',0.988235294117647,1.,0.266666666666667);
#19376=COLOUR_RGB('Dark Blue',0.08,0.2,0.34);
#19377=FILL_AREA_STYLE_COLOUR('',#19376);
#19378=FILL_AREA_STYLE('',(#19377));
#19379=SURFACE_STYLE_FILL_AREA(#19378);
#19380=SURFACE_SIDE_STYLE('',(#19379));
#19381=SURFACE_STYLE_USAGE(.BOTH.,#19380);
#19382=PRESENTATION_STYLE_ASSIGNMENT((#19381));
#19383=COLOUR_RGB('Light Blue',0.38,0.62,0.78);
#19384=FILL_AREA_STYLE_COLOUR('',#19383);
#19385=FILL_AREA_STYLE('',(#19384));
#19386=SURFACE_STYLE_FILL_AREA(#19385);
#19387=SURFACE_SIDE_STYLE('',(#19386));
#19388=SURFACE_STYLE_USAGE(.BOTH.,#19387);
#19389=PRESENTATION_STYLE_ASSIGNMENT((#19388));
#19390=COLOUR_RGB('Sky Blue',0.24,0.69,0.87);
#19391=FILL_AREA_STYLE_COLOUR('',#19390);
#19392=FILL_AREA_STYLE('',(#19391));
#19393=SURFACE_STYLE_FILL_AREA(#19392);
#19394=SURFACE_SIDE_STYLE('',(#19393));
#19395=SURFACE_STYLE_USAGE(.BOTH.,#19394);
#19396=PRESENTATION_STYLE_ASSIGNMENT((#19395));
#19397=COLOUR_RGB('Grey',0.48,0.52,0.57);
#19398=FILL_AREA_STYLE_COLOUR('',#19397);
#19399=FILL_AREA_STYLE('',(#19398));
#19400=SURFACE_STYLE_FILL_AREA(#19399);
#19401=SURFACE_SIDE_STYLE('',(#19400));
#19402=SURFACE_STYLE_USAGE(.BOTH.,#19401);
#19403=PRESENTATION_STYLE_ASSIGNMENT((#19402));
#19404=COLOUR_RGB('Black',0.12,0.14,0.17);
#19405=FILL_AREA_STYLE_COLOUR('',#19404);
#19406=FILL_AREA_STYLE('',(#19405));
#19407=SURFACE_STYLE_FILL_AREA(#19406);
#19408=SURFACE_SIDE_STYLE('',(#19407));
#19409=SURFACE_STYLE_USAGE(.BOTH.,#19408);
#19410=PRESENTATION_STYLE_ASSIGNMENT((#19409));
#19411=COLOUR_RGB('Off White',0.89,0.88,0.83);
#19412=FILL_AREA_STYLE_COLOUR('',#19411);
#19413=FILL_AREA_STYLE('',(#19412));
#19414=SURFACE_STYLE_FILL_AREA(#19413);
#19415=SURFACE_SIDE_STYLE('',(#19414));
#19416=SURFACE_STYLE_USAGE(.BOTH.,#19415);
#19417=PRESENTATION_STYLE_ASSIGNMENT((#19416));
ENDSEC;
END-ISO-10303-21;
